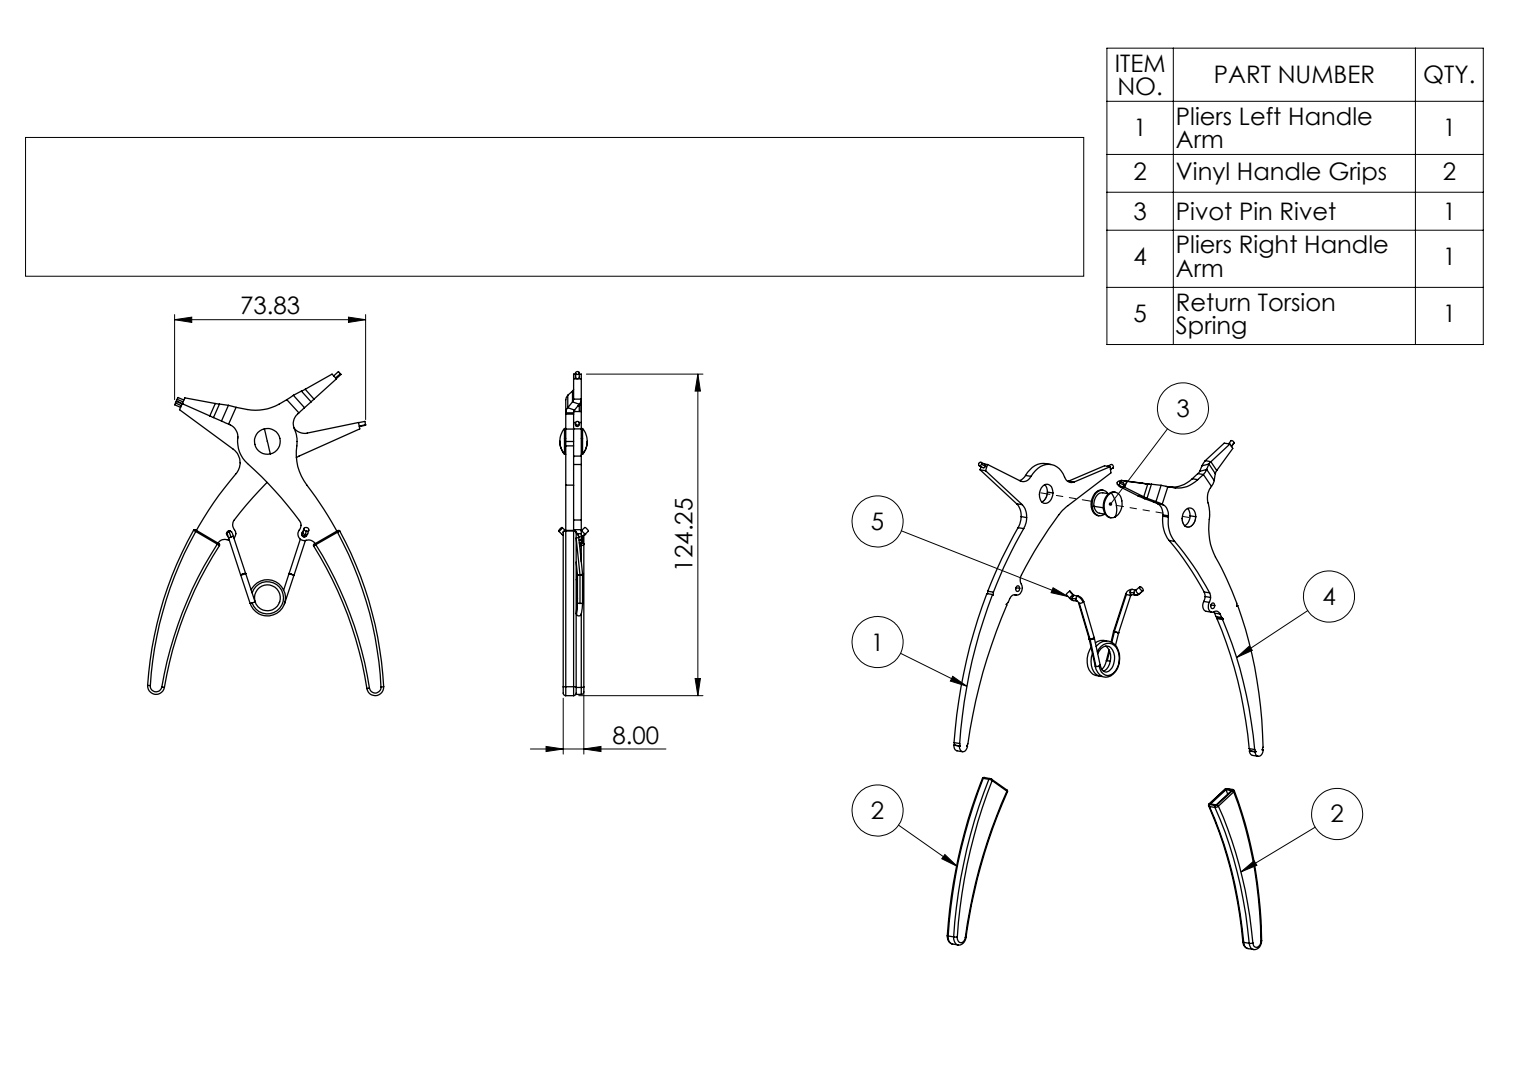
ISO-10303-21;
HEADER;
FILE_DESCRIPTION (('STEP AP214'),
    '1' );
FILE_NAME ('MAS-689',
    '2026-10-09T15:01:35',
    ( '' ),
    ( '' ),
    'SwSTEP 2.0',
    'SolidWorks 2026',
    '' );
FILE_SCHEMA (( 'AUTOMOTIVE_DESIGN' ));
ENDSEC;

DATA;
#1 = ORIENTED_EDGE ( 'NONE', *, *, #451, .F. ) ;
#2 = CIRCLE ( 'NONE', #2039, 3.300000000000002931 ) ;
#3 = DIRECTION ( 'NONE',  ( -5.715354789860003484E-18, -9.999836672264337477E-16, 1.000000000000000000 ) ) ;
#4 = DIRECTION ( 'NONE',  ( -5.715354789860003484E-18, -9.999836672264337477E-16, 1.000000000000000000 ) ) ;
#5 = EDGE_CURVE ( 'NONE', #1930, #3517, #6589, .T. ) ;
#6 = CARTESIAN_POINT ( 'NONE',  ( -2.243961179877913104, -65.88814609558559710, 1.271710548130833951 ) ) ;
#7 = VECTOR ( 'NONE', #4583, 1000.000000000000227 ) ;
#8 = CARTESIAN_POINT ( 'NONE',  ( 7.059059989562619819, -58.43975188330606585, -0.3221438859163246460 ) ) ;
#9 = CARTESIAN_POINT ( 'NONE',  ( -105.7473861751082040, -118.0666774205683822, -1.188285581044112860E-13 ) ) ;
#10 = ORIENTED_EDGE ( 'NONE', *, *, #1499, .F. ) ;
#11 = CARTESIAN_POINT ( 'NONE',  ( 39.48483786921892857, -95.33781693134928048, -9.497611030973018842E-14 ) ) ;
#12 = CARTESIAN_POINT ( 'NONE',  ( 1.714606436958001585E-17, 2.999951001679301835E-15, -3.000000000000000888 ) ) ;
#13 = CARTESIAN_POINT ( 'NONE',  ( 37.74350889372263396, 7.597106414893625370, -1.944871132915118705 ) ) ;
#14 = CARTESIAN_POINT ( 'NONE',  ( 10.02759472486470926, 5.630039434485818894, -2.999999999999995115 ) ) ;
#15 = EDGE_CURVE ( 'NONE', #320, #2542, #2080, .T. ) ;
#16 = CARTESIAN_POINT ( 'NONE',  ( 2.533447467746755333, -55.76293992159236979, -0.1309777151760100067 ) ) ;
#17 = CARTESIAN_POINT ( 'NONE',  ( -31.91091272472834817, 16.82560631625344172, 0.006154456448481410852 ) ) ;
#18 = FACE_OUTER_BOUND ( 'NONE', #7281, .T. ) ;
#19 = CIRCLE ( 'NONE', #5075, 1.000000000000001110 ) ;
#20 = PRODUCT_RELATED_PRODUCT_CATEGORY ( 'part', '', ( #4771 ) ) ;
#21 = ORIENTED_EDGE ( 'NONE', *, *, #345, .T. ) ;
#22 = ORIENTED_EDGE ( 'NONE', *, *, #4795, .T. ) ;
#23 = LINE ( 'NONE', #5799, #7366 ) ;
#24 = AXIS2_PLACEMENT_3D ( 'NONE', #2832, #2306, #6237 ) ;
#25 = AXIS2_PLACEMENT_3D ( 'NONE', #4428, #5501, #4998 ) ;
#26 = LINE ( 'NONE', #2324, #1475 ) ;
#27 = EDGE_CURVE ( 'NONE', #7442, #6679, #395, .T. ) ;
#28 = ADVANCED_FACE ( 'NONE', ( #2146 ), #5063, .T. ) ;
#29 = CARTESIAN_POINT ( 'NONE',  ( -6.272953878096410030, -61.45586155529391448, 1.493064301322690968 ) ) ;
#30 = CARTESIAN_POINT ( 'NONE',  ( 27.63595919327375938, -34.25856858997740062, -0.5081525913518375459 ) ) ;
#31 = CARTESIAN_POINT ( 'NONE',  ( 1.597826897138040048, -55.24069855439622501, 0.3109211183784004184 ) ) ;
#32 = CIRCLE ( 'NONE', #2308, 1.000000000000001110 ) ;
#33 = ORIENTED_EDGE ( 'NONE', *, *, #2628, .F. ) ;
#34 = AXIS2_PLACEMENT_3D ( 'NONE', #6184, #972, #7294 ) ;
#35 = FACE_OUTER_BOUND ( 'NONE', #4506, .T. ) ;
#36 = CARTESIAN_POINT ( 'NONE',  ( -15.08175531864075047, -34.71610473016205134, -5.729623873133089518 ) ) ;
#37 = AXIS2_PLACEMENT_3D ( 'NONE', #1867, #698, #7061 ) ;
#38 = EDGE_CURVE ( 'NONE', #489, #1005, #19, .T. ) ;
#39 = CARTESIAN_POINT ( 'NONE',  ( 9.311407240687648468, -51.41373841511902043, -1.002481404894999928 ) ) ;
#40 = AXIS2_PLACEMENT_3D ( 'NONE', #4287, #3708, #845 ) ;
#41 = CARTESIAN_POINT ( 'NONE',  ( -7.922926035662746003, 12.41525034409755612, 2.701156757981117984 ) ) ;
#42 = CYLINDRICAL_SURFACE ( 'NONE', #5055, 2.999999999999999556 ) ;
#43 = FILL_AREA_STYLE_COLOUR ( '', #963 ) ;
#44 = AXIS2_PLACEMENT_3D ( 'NONE', #1509, #3865, #2736 ) ;
#45 = ORIENTED_EDGE ( 'NONE', *, *, #3432, .T. ) ;
#46 = ORIENTED_EDGE ( 'NONE', *, *, #4272, .T. ) ;
#47 = AXIS2_PLACEMENT_3D ( 'NONE', #6946, #1636, #2269 ) ;
#48 = AXIS2_PLACEMENT_3D ( 'NONE', #1305, #1866, #2469 ) ;
#49 = DIRECTION ( 'NONE',  ( 5.715354789845005112E-18, 9.999836672264339449E-16, -1.000000000000000000 ) ) ;
#50 = AXIS2_PLACEMENT_3D ( 'NONE', #2705, #5732, #561 ) ;
#51 = SURFACE_STYLE_USAGE ( .BOTH. , #5819 ) ;
#52 = DIRECTION ( 'NONE',  ( 0.000000000000000000, -1.000000000000000000, -9.973300763855647239E-16 ) ) ;
#53 = CARTESIAN_POINT ( 'NONE',  ( -28.22553731214382111, -35.79092421365019305, -3.595165860846261460E-14 ) ) ;
#54 = CARTESIAN_POINT ( 'NONE',  ( -1.794944750655344867, -54.19869589391355191, -2.224588173883939035 ) ) ;
#55 = CARTESIAN_POINT ( 'NONE',  ( -13.19674249314596892, -2.997380612392111843, -3.000000000000003997 ) ) ;
#56 = VECTOR ( 'NONE', #5489, 1000.000000000000000 ) ;
#57 = EDGE_LOOP ( 'NONE', ( #3083, #4276, #3063, #5016, #4331, #6608 ) ) ;
#58 = CARTESIAN_POINT ( 'NONE',  ( -15.00216760413269945, 6.625337177075938833, -3.299999999999993161 ) ) ;
#59 = CARTESIAN_POINT ( 'NONE',  ( -14.70408710852078116, -35.66654345889202204, -3.000000000000036415 ) ) ;
#60 = CARTESIAN_POINT ( 'NONE',  ( 17.88843813672053074, -40.41242482140540204, -4.025211077939831437E-14 ) ) ;
#61 = DIRECTION ( 'NONE',  ( -0.9999836672264333925, 0.005715354789844476896, 0.000000000000000000 ) ) ;
#62 = CARTESIAN_POINT ( 'NONE',  ( 3.116905194451685013, -55.41725085606579171, 2.344137946175070653 ) ) ;
#63 = DIRECTION ( 'NONE',  ( -5.715354789860003484E-18, -9.999836672264337477E-16, 1.000000000000000000 ) ) ;
#64 = CARTESIAN_POINT ( 'NONE',  ( 43.95774332523846795, -95.00278575785266355, -9.454242944073598665E-14 ) ) ;
#65 = ORIENTED_EDGE ( 'NONE', *, *, #2017, .F. ) ;
#66 = ORIENTED_EDGE ( 'NONE', *, *, #4521, .T. ) ;
#67 = ORIENTED_EDGE ( 'NONE', *, *, #4872, .T. ) ;
#68 = ADVANCED_FACE ( 'NONE', ( #2687 ), #435, .T. ) ;
#69 = CARTESIAN_POINT ( 'NONE',  ( 18.49916120972752154, -39.46430250869199341, 3.499999999999960476 ) ) ;
#70 = VERTEX_POINT ( 'NONE', #2112 ) ;
#71 = CARTESIAN_POINT ( 'NONE',  ( 1.531562167974070077, -54.12800115838471271, -2.047325108518057935 ) ) ;
#72 = CARTESIAN_POINT ( 'NONE',  ( 26.87031364676133194, -34.69479876584122024, -0.5000000000000345279 ) ) ;
#73 = CARTESIAN_POINT ( 'NONE',  ( 3.016248221826935083, -64.97666327952782694, -3.135076956698916728 ) ) ;
#74 = VERTEX_POINT ( 'NONE', #2232 ) ;
#75 = VERTEX_POINT ( 'NONE', #4424 ) ;
#76 = EDGE_CURVE ( 'NONE', #70, #4585, #6096, .T. ) ;
#77 = EDGE_CURVE ( 'NONE', #427, #2020, #919, .T. ) ;
#78 =( NAMED_UNIT ( * ) SI_UNIT ( $, .STERADIAN. ) SOLID_ANGLE_UNIT ( ) );
#79 = CARTESIAN_POINT ( 'NONE',  ( 12.48153656191966476, 18.70005575237079043, -2.479608496603234347 ) ) ;
#80 = CARTESIAN_POINT ( 'NONE',  ( 8.409045811045761099, -50.95764513735950629, -2.495037190209991707 ) ) ;
#81 = DIRECTION ( 'NONE',  ( -5.715354789845005112E-18, -9.999836672264339449E-16, 1.000000000000000000 ) ) ;
#82 = DIRECTION ( 'NONE',  ( -0.9721221936972339606, -0.2344748185227520099, 0.000000000000000000 ) ) ;
#83 = LINE ( 'NONE', #2969, #2404 ) ;
#84 = EDGE_CURVE ( 'NONE', #5434, #6822, #3844, .T. ) ;
#85 = CARTESIAN_POINT ( 'NONE',  ( -4.132930949989339631, -63.16624423302310021, 2.163545901557570428 ) ) ;
#86 = DIRECTION ( 'NONE',  ( -0.5224671166576538850, 0.8526594349512809368, 0.000000000000000000 ) ) ;
#87 = FACE_OUTER_BOUND ( 'NONE', #3155, .T. ) ;
#88 = CYLINDRICAL_SURFACE ( 'NONE', #3600, 147.0000000000000284 ) ;
#89 = VERTEX_POINT ( 'NONE', #7308 ) ;
#90 = ADVANCED_FACE ( 'NONE', ( #990 ), #3285, .T. ) ;
#91 = CARTESIAN_POINT ( 'NONE',  ( 18.31438873653245381, -40.15745658308031807, 3.873766277856072193 ) ) ;
#92 = CARTESIAN_POINT ( 'NONE',  ( 9.769309212388114005, 25.48802373141157673, -2.993845543551514776 ) ) ;
#93 = FACE_OUTER_BOUND ( 'NONE', #5404, .T. ) ;
#94 = CARTESIAN_POINT ( 'NONE',  ( -2.961840227416660198, -65.56364223063081909, 1.283932781279834900 ) ) ;
#95 = CARTESIAN_POINT ( 'NONE',  ( -1.892846266465454841, -54.28526762408564110, -0.1610563749503846620 ) ) ;
#96 = CARTESIAN_POINT ( 'NONE',  ( 30.52077159997833533, 5.488396937353885896, -1.499999999999994893 ) ) ;
#97 = ORIENTED_EDGE ( 'NONE', *, *, #2305, .F. ) ;
#98 = ORIENTED_EDGE ( 'NONE', *, *, #6789, .F. ) ;
#99 =( REPRESENTATION_RELATIONSHIP ('NONE','NONE', #3195, #2136 ) REPRESENTATION_RELATIONSHIP_WITH_TRANSFORMATION ( #3447 )SHAPE_REPRESENTATION_RELATIONSHIP( ) );
#100 = DIRECTION ( 'NONE',  ( -0.9999836672264332815, 0.005715354789859956701, 0.000000000000000000 ) ) ;
#101 = PLANE ( 'NONE',  #156 ) ;
#102 = CARTESIAN_POINT ( 'NONE',  ( 2.906897738665179975, -66.25564029441702019, 0.8681355557765302322 ) ) ;
#103 = DIRECTION ( 'NONE',  ( 0.2223191033124284066, 0.6712482523644728305, 0.7071067811865467956 ) ) ;
#104 = EDGE_CURVE ( 'NONE', #5945, #4359, #7121, .T. ) ;
#105 = ORIENTED_EDGE ( 'NONE', *, *, #119, .T. ) ;
#106 = VERTEX_POINT ( 'NONE', #6746 ) ;
#107 = CARTESIAN_POINT ( 'NONE',  ( 27.99155020439382469, -34.64269665048638558, -3.446982116472166490E-14 ) ) ;
#108 = DIRECTION ( 'NONE',  ( 0.2344748185227520099, -0.9721221936972339606, 0.000000000000000000 ) ) ;
#109 = CARTESIAN_POINT ( 'NONE',  ( 5.682346379326408403, -62.38461083188095557, -3.511065069215000278 ) ) ;
#110 = DIRECTION ( 'NONE',  ( -0.9721221936972339606, -0.2344748185227520099, 0.000000000000000000 ) ) ;
#111 = EDGE_CURVE ( 'NONE', #70, #3385, #1232, .T. ) ;
#112 = EDGE_CURVE ( 'NONE', #2053, #3816, #7103, .T. ) ;
#113 = CARTESIAN_POINT ( 'NONE',  ( 1.437675307311687245, -54.36893612802973763, 0.01823407963783662405 ) ) ;
#114 = ORIENTED_EDGE ( 'NONE', *, *, #332, .F. ) ;
#115 = PRODUCT_RELATED_PRODUCT_CATEGORY ( 'part', '', ( #196 ) ) ;
#116 = CARTESIAN_POINT ( 'NONE',  ( 4.115360779042029904, -63.19255852436059229, -2.695130055691413506 ) ) ;
#117 = CARTESIAN_POINT ( 'NONE',  ( -20.16480223318149356, 14.61937842657788345, -2.993845543551524990 ) ) ;
#118 = CARTESIAN_POINT ( 'NONE',  ( 9.769309212388092689, 25.48802373141157318, 0.006154456448490518150 ) ) ;
#119 = EDGE_CURVE ( 'NONE', #427, #4029, #5685, .T. ) ;
#120 = ADVANCED_FACE ( 'NONE', ( #5785 ), #4047, .F. ) ;
#121 = CARTESIAN_POINT ( 'NONE',  ( 2.653562475325737857, -65.64394347387724338, 0.9832085570212988346 ) ) ;
#122 = AXIS2_PLACEMENT_3D ( 'NONE', #4190, #238, #5631 ) ;
#123 = VERTEX_POINT ( 'NONE', #4619 ) ;
#124 = CARTESIAN_POINT ( 'NONE',  ( -5.765066695091211280, -62.35357808832723947, 3.545399627195713332 ) ) ;
#125 = AXIS2_PLACEMENT_3D ( 'NONE', #6895, #3541, #4566 ) ;
#126 = DIRECTION ( 'NONE',  ( -0.2344748185227520376, 0.9721221936972340716, 0.000000000000000000 ) ) ;
#127 = CARTESIAN_POINT ( 'NONE',  ( 1.275220786007323914, -54.66846601681689322, 0.1350250863793004130 ) ) ;
#128 = CARTESIAN_POINT ( 'NONE',  ( 2.080482015124565098, -66.54183146390657555, -1.221303033644861813 ) ) ;
#129 = DIRECTION ( 'NONE',  ( -1.602374898470634869E-16, 1.442524254523139935E-17, 1.000000000000000000 ) ) ;
#130 = ORIENTED_EDGE ( 'NONE', *, *, #2556, .T. ) ;
#131 = ORIENTED_EDGE ( 'NONE', *, *, #84, .F. ) ;
#132 = VECTOR ( 'NONE', #4275, 1000.000000000000000 ) ;
#133 = FACE_OUTER_BOUND ( 'NONE', #7338, .T. ) ;
#134 = CARTESIAN_POINT ( 'NONE',  ( -4.860610968486169803, -1.172374092613760022, 3.500000000000000000 ) ) ;
#135 = CARTESIAN_POINT ( 'NONE',  ( -6.814417183322500016, -58.48210382454914935, -0.1019614231452001113 ) ) ;
#136 = CARTESIAN_POINT ( 'NONE',  ( 27.99155020439386377, -34.64269665048637137, -4.257530847521587323E-14 ) ) ;
#137 = ORIENTED_EDGE ( 'NONE', *, *, #2521, .F. ) ;
#138 = VERTEX_POINT ( 'NONE', #4690 ) ;
#139 = ORIENTED_EDGE ( 'NONE', *, *, #2264, .T. ) ;
#140 = EDGE_CURVE ( 'NONE', #6822, #6113, #1025, .T. ) ;
#141 =( NAMED_UNIT ( * ) SI_UNIT ( $, .STERADIAN. ) SOLID_ANGLE_UNIT ( ) );
#142 = PLANE ( 'NONE',  #2794 ) ;
#143 = DIRECTION ( 'NONE',  ( -0.9721221936972339606, -0.2344748185227520099, 0.000000000000000000 ) ) ;
#144 = DIRECTION ( 'NONE',  ( 0.2223157560262044585, -0.6712493609847989262, 0.7071067811865449082 ) ) ;
#145 = CARTESIAN_POINT ( 'NONE',  ( 30.52077159997833533, 5.488396937353885896, -1.499999999999994893 ) ) ;
#146 = CIRCLE ( 'NONE', #7235, 1.000000000000000888 ) ;
#147 = CIRCLE ( 'NONE', #6885, 6.299999999999998934 ) ;
#148 = AXIS2_PLACEMENT_3D ( 'NONE', #6165, #6059, #1524 ) ;
#149 = CARTESIAN_POINT ( 'NONE',  ( -5.163597282883630513, -63.01551968439245144, 3.580859834736030312 ) ) ;
#150 = VECTOR ( 'NONE', #1771, 1000.000000000000227 ) ;
#151 = VECTOR ( 'NONE', #4371, 999.9999999999998863 ) ;
#152 = CARTESIAN_POINT ( 'NONE',  ( 0.000000000000000000, 0.000000000000000000, 2.544444444444450060 ) ) ;
#153 = CARTESIAN_POINT ( 'NONE',  ( -4.969000869418408683, -63.40403411709974790, -2.714243491562927879 ) ) ;
#154 = CARTESIAN_POINT ( 'NONE',  ( -2.104778383727555102, -66.59261038346899397, 1.133408834283370137 ) ) ;
#155 = DIRECTION ( 'NONE',  ( -0.9999836672264332815, 0.005715354789859956701, 0.000000000000000000 ) ) ;
#156 = AXIS2_PLACEMENT_3D ( 'NONE', #5801, #629, #4670 ) ;
#157 = CIRCLE ( 'NONE', #1946, 1.000000000000000444 ) ;
#158 = EDGE_LOOP ( 'NONE', ( #2587, #5336, #2767, #4336, #3455, #7221 ) ) ;
#159 = PRODUCT_DEFINITION_FORMATION_WITH_SPECIFIED_SOURCE ( 'ANY', '', #255, .NOT_KNOWN. ) ;
#160 = CARTESIAN_POINT ( 'NONE',  ( -28.26642576027046516, -36.90973657692984489, -3.000000000000037748 ) ) ;
#161 = EDGE_CURVE ( 'NONE', #2317, #4548, #3992, .T. ) ;
#162 = EDGE_CURVE ( 'NONE', #6490, #232, #2554, .T. ) ;
#163 = LINE ( 'NONE', #7048, #1585 ) ;
#164 = AXIS2_PLACEMENT_3D ( 'NONE', #6562, #6008, #5019 ) ;
#165 = CARTESIAN_POINT ( 'NONE',  ( 12.40979888490706706, -30.61452125107581068, 2.999999999999969802 ) ) ;
#166 = DIRECTION ( 'NONE',  ( 5.715354789845005112E-18, 9.999836672264339449E-16, -1.000000000000000000 ) ) ;
#167 = CARTESIAN_POINT ( 'NONE',  ( -6.199032880790720235, -61.56120177486793210, 3.556545127952429830 ) ) ;
#168 = AXIS2_PLACEMENT_3D ( 'NONE', #4159, #3722, #2491 ) ;
#169 = CIRCLE ( 'NONE', #2691, 147.0000000000000000 ) ;
#170 = CARTESIAN_POINT ( 'NONE',  ( 5.465222000274489567, -57.03231251543625291, 0.2812537129946697800 ) ) ;
#171 = CARTESIAN_POINT ( 'NONE',  ( -16.51707533432788111, -40.85914143033993895, -3.000000000000041744 ) ) ;
#172 = ORIENTED_EDGE ( 'NONE', *, *, #3864, .T. ) ;
#173 = ORIENTED_EDGE ( 'NONE', *, *, #526, .F. ) ;
#174 = ORIENTED_EDGE ( 'NONE', *, *, #2963, .T. ) ;
#175 = EDGE_CURVE ( 'NONE', #6662, #3589, #2174, .T. ) ;
#176 = CIRCLE ( 'NONE', #6665, 0.7499999999999893419 ) ;
#177 = DIRECTION ( 'NONE',  ( -0.9492883822130750993, 0.3144066910790588865, 0.000000000000000000 ) ) ;
#178 = PLANE ( 'NONE',  #37 ) ;
#179 = CARTESIAN_POINT ( 'NONE',  ( 5.575556491096470779, -57.10417477796837460, -1.782215851858570010 ) ) ;
#180 = CARTESIAN_POINT ( 'NONE',  ( 9.311407240687648468, -51.41373841511900622, -2.502481404895003259 ) ) ;
#181 = VERTEX_POINT ( 'NONE', #5749 ) ;
#182 = ORIENTED_EDGE ( 'NONE', *, *, #4904, .T. ) ;
#183 = ORIENTED_EDGE ( 'NONE', *, *, #2628, .T. ) ;
#184 = VERTEX_POINT ( 'NONE', #578 ) ;
#185 =( LENGTH_UNIT ( ) NAMED_UNIT ( * ) SI_UNIT ( .MILLI., .METRE. ) );
#186 = CARTESIAN_POINT ( 'NONE',  ( 3.888488774788935842, 0.9378992740910084835, 3.000000000000000000 ) ) ;
#187 = CARTESIAN_POINT ( 'NONE',  ( 27.98760434640042050, 26.43260972569849443, -1.493845543551990174 ) ) ;
#188 = DIRECTION ( 'NONE',  ( 0.3128416502900965290, -0.9445788350777319931, 0.09950339776592478924 ) ) ;
#189 = CARTESIAN_POINT ( 'NONE',  ( -3.569041007005829602, -65.81017109676685095, 3.284668648760890264 ) ) ;
#190 = PLANE ( 'NONE',  #25 ) ;
#191 = ORIENTED_EDGE ( 'NONE', *, *, #892, .F. ) ;
#192 = CARTESIAN_POINT ( 'NONE',  ( -2.392055737067099841, -65.19778216667813808, -1.190937291917544050 ) ) ;
#193 = CARTESIAN_POINT ( 'NONE',  ( -14.49899450467539985, -35.75040780681265318, -0.4662714048949997969 ) ) ;
#194 = DIRECTION ( 'NONE',  ( 9.251858538542970644E-15, 2.775557561562891351E-14, 1.000000000000000000 ) ) ;
#195 = CARTESIAN_POINT ( 'NONE',  ( -3.055077159899213690, -65.35589988530520600, -0.7735514844714416194 ) ) ;
#196 = PRODUCT ( 'Pliers Right Handle Arm', 'Pliers Right Handle Arm', '', ( #6070 ) ) ;
#197 = CARTESIAN_POINT ( 'NONE',  ( 3.257640280419950241, -66.06664283717124420, -1.252360977842533751 ) ) ;
#198 = EDGE_CURVE ( 'NONE', #3368, #5232, #6974, .T. ) ;
#199 = ORIENTED_EDGE ( 'NONE', *, *, #978, .F. ) ;
#200 = DIRECTION ( 'NONE',  ( 0.9999836672264332815, -0.005715354789844959149, 0.000000000000000000 ) ) ;
#201 = DIRECTION ( 'NONE',  ( 0.8552446107963830313, 0.5182245224839744369, 5.231040848230092092E-16 ) ) ;
#202 = CYLINDRICAL_SURFACE ( 'NONE', #2445, 0.5000000000000022204 ) ;
#203 = CARTESIAN_POINT ( 'NONE',  ( -3.235261603508409856, -66.01500717273368934, 1.164464255201294929 ) ) ;
#204 = CARTESIAN_POINT ( 'NONE',  ( -5.227302941343250353, -58.92678856866081105, -0.2192372590660296439 ) ) ;
#205 = CARTESIAN_POINT ( 'NONE',  ( -6.490403473174280791, -62.28500686936251185, 3.403714661497959870 ) ) ;
#206 = EDGE_CURVE ( 'NONE', #2991, #6689, #4958, .T. ) ;
#207 = CARTESIAN_POINT ( 'NONE',  ( -17.21006346072928750, 13.86884027412869180, -2.230393353321906247 ) ) ;
#208 = ORIENTED_EDGE ( 'NONE', *, *, #252, .F. ) ;
#209 = ADVANCED_FACE ( 'NONE', ( #688 ), #379, .F. ) ;
#210 = VERTEX_POINT ( 'NONE', #2865 ) ;
#211 = EDGE_LOOP ( 'NONE', ( #3520, #3050, #137, #3824 ) ) ;
#212 = VERTEX_POINT ( 'NONE', #11 ) ;
#213 = DIRECTION ( 'NONE',  ( -5.715354789845005112E-18, -9.999836672264339449E-16, 1.000000000000000000 ) ) ;
#214 = CARTESIAN_POINT ( 'NONE',  ( 14.18471095241310032, -36.69976849081635351, 0.4975185951050001831 ) ) ;
#215 = CARTESIAN_POINT ( 'NONE',  ( -1.756031117750795234, -65.59594772693552045, 1.371125244074580030 ) ) ;
#216 = VERTEX_POINT ( 'NONE', #6910 ) ;
#217 = EDGE_CURVE ( 'NONE', #3483, #2618, #2661, .T. ) ;
#218 = ORIENTED_EDGE ( 'NONE', *, *, #3975, .F. ) ;
#219 = EDGE_LOOP ( 'NONE', ( #5454, #1451, #6530, #3936 ) ) ;
#220 = ORIENTED_EDGE ( 'NONE', *, *, #5909, .F. ) ;
#221 = DIRECTION ( 'NONE',  ( 0.1200071523045019850, -0.5808948794702039065, -0.8050834878452428622 ) ) ;
#222 = CARTESIAN_POINT ( 'NONE',  ( 27.68174825049008803, -37.24611774345110859, -3.729655473350135253E-14 ) ) ;
#223 = DIRECTION ( 'NONE',  ( 0.4039838799357178822, 0.9147661038495488173, -2.999999999999999208E-14 ) ) ;
#224 = CARTESIAN_POINT ( 'NONE',  ( -6.308476396955129850, -59.14191327212131455, -0.5142043607924547954 ) ) ;
#225 = ORIENTED_EDGE ( 'NONE', *, *, #2234, .T. ) ;
#226 = EDGE_CURVE ( 'NONE', #477, #1089, #6052, .T. ) ;
#227 = DIRECTION ( 'NONE',  ( 5.715354789845004342E-18, 9.999836672264337477E-16, -1.000000000000000000 ) ) ;
#228 = CARTESIAN_POINT ( 'NONE',  ( -5.725946002089390419, -61.92844332740136792, 1.548851071596535123 ) ) ;
#229 =( NAMED_UNIT ( * ) SI_UNIT ( $, .STERADIAN. ) SOLID_ANGLE_UNIT ( ) );
#230 = DIRECTION ( 'NONE',  ( -0.9999836672264333925, 0.005715354789844960016, 0.000000000000000000 ) ) ;
#231 = CARTESIAN_POINT ( 'NONE',  ( 2.221695044209367698, -65.89517911169727427, -1.088420971642926727 ) ) ;
#232 = VERTEX_POINT ( 'NONE', #3010 ) ;
#233 = LINE ( 'NONE', #4722, #5692 ) ;
#234 = TOROIDAL_SURFACE ( 'NONE', #5408, 140.0000000000000000, 1.000000000000000000 ) ;
#235 = EDGE_CURVE ( 'NONE', #5505, #4310, #421, .T. ) ;
#236 = CARTESIAN_POINT ( 'NONE',  ( -19.02987527034469650, -39.22028924617138301, -3.000000000000040412 ) ) ;
#237 = CARTESIAN_POINT ( 'NONE',  ( 18.49916120972751088, -39.46430250869199341, -0.5000000000000393019 ) ) ;
#238 = DIRECTION ( 'NONE',  ( 0.6713653717953971256, -0.7411265327553914206, -1.050567784676125892E-15 ) ) ;
#239 = CARTESIAN_POINT ( 'NONE',  ( -6.429839020462739363, -63.58404662519255623, 2.770540757372710328 ) ) ;
#240 = CARTESIAN_POINT ( 'NONE',  ( -44.78727511552453677, -94.39397278840091587, -9.464840624037363205E-14 ) ) ;
#241 = EDGE_LOOP ( 'NONE', ( #2453, #5652, #2656, #1275 ) ) ;
#242 = ORIENTED_EDGE ( 'NONE', *, *, #3196, .T. ) ;
#243 = AXIS2_PLACEMENT_3D ( 'NONE', #3684, #2023, #7044 ) ;
#244 = CARTESIAN_POINT ( 'NONE',  ( -28.68093632328499965, 11.79168739492699913, -1.500000000001999956 ) ) ;
#245 = CARTESIAN_POINT ( 'NONE',  ( -105.7473861751082040, -118.0666774205683822, 2.999999999999881428 ) ) ;
#246 = CARTESIAN_POINT ( 'NONE',  ( -5.466570931786790766, -63.95713299600960511, -2.842748680216657942 ) ) ;
#247 = CARTESIAN_POINT ( 'NONE',  ( 2.831152723192955190, -54.81765481733766876, 0.09675599308719184943 ) ) ;
#248 = CIRCLE ( 'NONE', #4943, 5.000000000000001776 ) ;
#249 = ORIENTED_EDGE ( 'NONE', *, *, #5609, .F. ) ;
#250 = EDGE_LOOP ( 'NONE', ( #2222, #4590, #6016, #4607 ) ) ;
#251 = ORIENTED_EDGE ( 'NONE', *, *, #6437, .T. ) ;
#252 = EDGE_CURVE ( 'NONE', #1688, #1547, #147, .T. ) ;
#253 = EDGE_CURVE ( 'NONE', #4908, #2830, #5444, .T. ) ;
#254 = CARTESIAN_POINT ( 'NONE',  ( 23.12979183812720407, 24.32586137474685017, -8.815182418718713109 ) ) ;
#255 = PRODUCT ( 'Return Torsion Spring', 'Return Torsion Spring', '', ( #964 ) ) ;
#256 = FACE_BOUND ( 'NONE', #7433, .T. ) ;
#257 = CARTESIAN_POINT ( 'NONE',  ( 12.34225220476766438, -34.27182074065601114, 2.999999999999965805 ) ) ;
#258 = CARTESIAN_POINT ( 'NONE',  ( -5.971666637568279867, -56.84728173661435591, 1.574849794282134896 ) ) ;
#259 = ORIENTED_EDGE ( 'NONE', *, *, #1801, .T. ) ;
#260 = DIRECTION ( 'NONE',  ( -0.6713653717953970146, 0.7411265327553913096, 7.633377738797892154E-16 ) ) ;
#261 = EDGE_CURVE ( 'NONE', #1236, #2830, #5625, .T. ) ;
#262 = CARTESIAN_POINT ( 'NONE',  ( 4.897692307440769888, -62.02301377339387756, -1.765793165935516829 ) ) ;
#263 = CARTESIAN_POINT ( 'NONE',  ( 12.26605808802378661, -5.710507655519335479, -3.000000000000006661 ) ) ;
#264 = VECTOR ( 'NONE', #2040, 1000.000000000000000 ) ;
#265 = VECTOR ( 'NONE', #2707, 999.9999999999998863 ) ;
#266 = CYLINDRICAL_SURFACE ( 'NONE', #6602, 11.50000000000000178 ) ;
#267 = CARTESIAN_POINT ( 'NONE',  ( 3.367951392835606406, -65.15049214652208320, -1.167130348240442927 ) ) ;
#268 = ORIENTED_EDGE ( 'NONE', *, *, #1200, .T. ) ;
#269 = CIRCLE ( 'NONE', #6408, 140.0000000000000000 ) ;
#270 = CARTESIAN_POINT ( 'NONE',  ( -41.31559769795914150, -94.79889909491285493, -3.000000000000095923 ) ) ;
#271 = VECTOR ( 'NONE', #2311, 1000.000000000000000 ) ;
#272 = DIRECTION ( 'NONE',  ( 0.3128463504745285229, 0.9445772445362839997, 0.09950371902099811039 ) ) ;
#273 = DIRECTION ( 'NONE',  ( -0.4039838799357104993, -0.9147661038495521479, -3.619485620725444841E-16 ) ) ;
#274 = UNCERTAINTY_MEASURE_WITH_UNIT (LENGTH_MEASURE( 1.000000000000000082E-05 ), #185, 'distance_accuracy_value', 'NONE');
#275 = AXIS2_PLACEMENT_3D ( 'NONE', #245, #7168, #3592 ) ;
#276 = CARTESIAN_POINT ( 'NONE',  ( -3.156642594714314853, -54.82761582543010093, 1.871643660998590697 ) ) ;
#277 = AXIS2_PLACEMENT_3D ( 'NONE', #4931, #1502, #1047 ) ;
#278 = CARTESIAN_POINT ( 'NONE',  ( -1.626396133375414887, -53.66552156771879112, 1.839959185157149957 ) ) ;
#279 = DIRECTION ( 'NONE',  ( 0.000000000000000000, -0.7252570966694442678, 0.6884781359858920258 ) ) ;
#280 = ORIENTED_EDGE ( 'NONE', *, *, #2225, .T. ) ;
#281 = AXIS2_PLACEMENT_3D ( 'NONE', #1500, #409, #4895 ) ;
#282 = ORIENTED_EDGE ( 'NONE', *, *, #5430, .F. ) ;
#283 = ORIENTED_EDGE ( 'NONE', *, *, #2017, .T. ) ;
#284 = AXIS2_PLACEMENT_3D ( 'NONE', #2458, #4271, #126 ) ;
#285 = CARTESIAN_POINT ( 'NONE',  ( -15.07233531785332659, 13.90759097395377886, 2.236547809770392803 ) ) ;
#286 = CIRCLE ( 'NONE', #4504, 147.0000000000000284 ) ;
#287 = VECTOR ( 'NONE', #7438, 1000.000000000000000 ) ;
#288 = DIRECTION ( 'NONE',  ( 0.9986925448795970217, 0.05111947575938272093, 5.682652305652042775E-17 ) ) ;
#289 = CARTESIAN_POINT ( 'NONE',  ( 1.662636012147085118, -65.62619303409478277, -3.045852711070930141 ) ) ;
#290 = CARTESIAN_POINT ( 'NONE',  ( 4.774359225188401723, -64.47360709931102463, 0.6998940494460414996 ) ) ;
#291 = ORIENTED_EDGE ( 'NONE', *, *, #6437, .F. ) ;
#292 = ORIENTED_EDGE ( 'NONE', *, *, #6726, .T. ) ;
#293 = EDGE_CURVE ( 'NONE', #961, #6756, #1329, .T. ) ;
#294 = ORIENTED_EDGE ( 'NONE', *, *, #1501, .T. ) ;
#295 = ORIENTED_EDGE ( 'NONE', *, *, #5689, .F. ) ;
#296 = DIRECTION ( 'NONE',  ( 0.9492899500389736511, 0.3144019573014823488, 0.000000000000000000 ) ) ;
#297 = DIRECTION ( 'NONE',  ( -0.2023178344681509366, 0.9793199139485104787, 9.781476007338054812E-16 ) ) ;
#298 = CIRCLE ( 'NONE', #3775, 145.9999999999999716 ) ;
#299 = PLANE ( 'NONE',  #650 ) ;
#300 = CARTESIAN_POINT ( 'NONE',  ( 6.696612653858620590, -58.50870383553881737, 0.2496331057155200817 ) ) ;
#301 = EDGE_LOOP ( 'NONE', ( #225, #3972, #6636, #4802 ) ) ;
#302 = ADVANCED_FACE ( 'NONE', ( #3614 ), #3261, .F. ) ;
#303 = EDGE_CURVE ( 'NONE', #4768, #4244, #4606, .T. ) ;
#304 = EDGE_LOOP ( 'NONE', ( #2533, #3781, #4954, #1609 ) ) ;
#305 = DIRECTION ( 'NONE',  ( 5.715354789845005112E-18, 9.999836672264339449E-16, -1.000000000000000000 ) ) ;
#306 = CARTESIAN_POINT ( 'NONE',  ( -5.408997660349871062, -62.29959681528816873, 3.625047998704080232 ) ) ;
#307 = ORIENTED_EDGE ( 'NONE', *, *, #6778, .T. ) ;
#308 = DIRECTION ( 'NONE',  ( -5.715354789860003484E-18, -9.999836672264337477E-16, 1.000000000000000000 ) ) ;
#309 = CARTESIAN_POINT ( 'NONE',  ( -0.5318364440386327274, -66.20751837745356738, -3.028967907328838027 ) ) ;
#310 = EDGE_CURVE ( 'NONE', #1930, #1079, #233, .T. ) ;
#311 = ORIENTED_EDGE ( 'NONE', *, *, #217, .T. ) ;
#312 = CARTESIAN_POINT ( 'NONE',  ( 14.02750760687355935, -37.17441268192290238, 0.4975185951050001831 ) ) ;
#313 = CARTESIAN_POINT ( 'NONE',  ( 27.55235279947361349, -34.88166451341158592, 3.999999999999965361 ) ) ;
#314 = DIRECTION ( 'NONE',  ( 0.3128416502900965290, -0.9445788350777319931, 0.09950339776592478924 ) ) ;
#315 = DIRECTION ( 'NONE',  ( -0.4328040977884316520, 0.5819352847797604200, 0.6884997728872834788 ) ) ;
#316 = LINE ( 'NONE', #1518, #3268 ) ;
#317 = CARTESIAN_POINT ( 'NONE',  ( 6.075450823322679383, -63.85990335785957228, 0.5148622082158803570 ) ) ;
#318 = CARTESIAN_POINT ( 'NONE',  ( -95.86211798318534250, -102.0316339954322018, 3.999999999999897859 ) ) ;
#319 = ADVANCED_FACE ( 'NONE', ( #794 ), #822, .F. ) ;
#320 = VERTEX_POINT ( 'NONE', #758 ) ;
#321 = VERTEX_POINT ( 'NONE', #1855 ) ;
#322 = CARTESIAN_POINT ( 'NONE',  ( 15.39900769062488806, 3.181283097128406290, -2.999999999999997335 ) ) ;
#323 = FACE_OUTER_BOUND ( 'NONE', #1179, .T. ) ;
#324 = CARTESIAN_POINT ( 'NONE',  ( -4.747117373927349782, -63.10583374278928659, -0.4844647803776696016 ) ) ;
#325 = CARTESIAN_POINT ( 'NONE',  ( 6.103722004628568065, 22.16747290800961778, 2.236547809770398576 ) ) ;
#326 = CARTESIAN_POINT ( 'NONE',  ( -4.385465831998347497, -64.89496069624793506, 1.250664309176121813 ) ) ;
#327 = VERTEX_POINT ( 'NONE', #3117 ) ;
#328 = ORIENTED_EDGE ( 'NONE', *, *, #1145, .T. ) ;
#329 = ORIENTED_EDGE ( 'NONE', *, *, #1529, .F. ) ;
#330 =( NAMED_UNIT ( * ) PLANE_ANGLE_UNIT ( ) SI_UNIT ( $, .RADIAN. ) );
#331 = CARTESIAN_POINT ( 'NONE',  ( -18.51952944085035924, 14.44713361607367830, 0.4060579846639892909 ) ) ;
#332 = EDGE_CURVE ( 'NONE', #5680, #3331, #6168, .T. ) ;
#333 = LINE ( 'NONE', #6030, #1620 ) ;
#334 = CARTESIAN_POINT ( 'NONE',  ( -33.25476684253261794, 13.81160679460555940, -0.7499999999999977796 ) ) ;
#335 = CARTESIAN_POINT ( 'NONE',  ( 1.944327905822930136, -53.75057748617523856, 2.017748614706070143 ) ) ;
#336 = ORIENTED_EDGE ( 'NONE', *, *, #6986, .T. ) ;
#337 = FACE_OUTER_BOUND ( 'NONE', #6918, .T. ) ;
#338 = CARTESIAN_POINT ( 'NONE',  ( -1.512046953658800152, -54.18079592905042574, 1.959428465566195543 ) ) ;
#339 = EDGE_CURVE ( 'NONE', #4174, #2620, #4361, .T. ) ;
#340 = CYLINDRICAL_SURFACE ( 'NONE', #3356, 0.7500000000000000000 ) ;
#341 = DIRECTION ( 'NONE',  ( 5.715354789860003484E-18, 9.999836672264337477E-16, -1.000000000000000000 ) ) ;
#342 = ORIENTED_EDGE ( 'NONE', *, *, #3838, .T. ) ;
#343 = EDGE_CURVE ( 'NONE', #1942, #4478, #3077, .T. ) ;
#344 = CARTESIAN_POINT ( 'NONE',  ( 18.49916120972752509, -39.46430250869199341, 3.499999999999960476 ) ) ;
#345 = EDGE_CURVE ( 'NONE', #1893, #5033, #4794, .T. ) ;
#346 = CYLINDRICAL_SURFACE ( 'NONE', #4266, 3.300000000000001599 ) ;
#347 = DIRECTION ( 'NONE',  ( -0.8056443796264689539, 0.5923994712829191434, 5.877852522924718954E-16 ) ) ;
#348 = DIRECTION ( 'NONE',  ( -5.715354789845005112E-18, -9.999836672264339449E-16, 1.000000000000000000 ) ) ;
#349 = FACE_OUTER_BOUND ( 'NONE', #6871, .T. ) ;
#350 = CARTESIAN_POINT ( 'NONE',  ( 3.592758869166885471, -66.41582265024271692, 0.6922273147611399668 ) ) ;
#351 = DIRECTION ( 'NONE',  ( -5.715354789860003484E-18, -9.999836672264337477E-16, 1.000000000000000000 ) ) ;
#352 = AXIS2_PLACEMENT_3D ( 'NONE', #2407, #3501, #6969 ) ;
#353 = ORIENTED_EDGE ( 'NONE', *, *, #3724, .F. ) ;
#354 = VERTEX_POINT ( 'NONE', #1399 ) ;
#355 = ORIENTED_EDGE ( 'NONE', *, *, #4403, .T. ) ;
#356 = FACE_OUTER_BOUND ( 'NONE', #779, .T. ) ;
#357 = AXIS2_PLACEMENT_3D ( 'NONE', #1661, #431, #1029 ) ;
#358 = FACE_OUTER_BOUND ( 'NONE', #3624, .T. ) ;
#359 = CARTESIAN_POINT ( 'NONE',  ( -5.294444503516980483, -61.70453834742492916, -0.3952116983248150084 ) ) ;
#360 = FACE_OUTER_BOUND ( 'NONE', #2389, .T. ) ;
#361 = CARTESIAN_POINT ( 'NONE',  ( -6.248181790555211279, -60.49255085186674563, 1.512929826500920338 ) ) ;
#362 = CARTESIAN_POINT ( 'NONE',  ( -4.797760869400969241, -62.71499483963494015, 1.636667228454699696 ) ) ;
#363 = ORIENTED_EDGE ( 'NONE', *, *, #858, .F. ) ;
#364 = VERTEX_POINT ( 'NONE', #160 ) ;
#365 = EDGE_LOOP ( 'NONE', ( #2898, #4599, #960, #5000 ) ) ;
#366 = VECTOR ( 'NONE', #3433, 1000.000000000000000 ) ;
#367 =( NAMED_UNIT ( * ) PLANE_ANGLE_UNIT ( ) SI_UNIT ( $, .RADIAN. ) );
#368 = DIRECTION ( 'NONE',  ( 5.715354789845005112E-18, 9.999836672264339449E-16, -1.000000000000000000 ) ) ;
#369 = AXIS2_PLACEMENT_3D ( 'NONE', #2221, #569, #5170 ) ;
#370 = DIRECTION ( 'NONE',  ( -0.9999836672264335036, 0.005715354789845008589, 0.000000000000000000 ) ) ;
#371 = CARTESIAN_POINT ( 'NONE',  ( 6.135463341229070444, -63.36916140199613778, -1.604994752452352014 ) ) ;
#372 = ORIENTED_EDGE ( 'NONE', *, *, #5459, .F. ) ;
#373 = ORIENTED_EDGE ( 'NONE', *, *, #4079, .F. ) ;
#374 = ADVANCED_FACE ( 'NONE', ( #1915 ), #2901, .T. ) ;
#375 = CARTESIAN_POINT ( 'NONE',  ( 39.48483786921892857, -95.33781693134928048, 3.999999999999904521 ) ) ;
#376 = CARTESIAN_POINT ( 'NONE',  ( -18.51952944085035924, 14.44713361607365876, 0.4060579846639944535 ) ) ;
#377 = CARTESIAN_POINT ( 'NONE',  ( 15.08188723176695056, -33.99092340910145538, 5.072392329257909616 ) ) ;
#378 = DIRECTION ( 'NONE',  ( 0.000000000000000000, -0.7252570966694443788, 0.6884781359858918037 ) ) ;
#379 = CONICAL_SURFACE ( 'NONE', #3862, 0.7499999999999865663, 1.029744258676651425 ) ;
#380 = VERTEX_POINT ( 'NONE', #6559 ) ;
#381 = EDGE_CURVE ( 'NONE', #2927, #5703, #3139, .T. ) ;
#382 = B_SPLINE_CURVE_WITH_KNOTS ( 'NONE', 3,
 ( #5287, #6445, #2450, #5362, #4685, #5889 ),
 .UNSPECIFIED., .F., .F.,
 ( 4, 2, 4 ),
 ( 0.000000000000000000, 0.5000000000000000000, 1.000000000000000000 ),
 .UNSPECIFIED. ) ;
#383 = VECTOR ( 'NONE', #1135, 1000.000000000000000 ) ;
#384 = DIRECTION ( 'NONE',  ( 0.9999836672264332815, -0.005715354789859936752, 0.000000000000000000 ) ) ;
#385 = CARTESIAN_POINT ( 'NONE',  ( 7.541408601728222472, 23.46983215994270822, -2.230393353321886263 ) ) ;
#386 = CARTESIAN_POINT ( 'NONE',  ( -105.7473861751082040, -118.0666774205683822, 2.999999999999881428 ) ) ;
#387 = CARTESIAN_POINT ( 'NONE',  ( -95.86211798318534250, -102.0316339954322018, 2.999999999999897859 ) ) ;
#388 = CARTESIAN_POINT ( 'NONE',  ( -6.381106047699259598, -62.60757382768967716, 3.386766328596300113 ) ) ;
#389 = DIRECTION ( 'NONE',  ( 0.000000000000000000, 0.000000000000000000, -1.000000000000000000 ) ) ;
#390 = AXIS2_PLACEMENT_3D ( 'NONE', #1613, #3079, #7288 ) ;
#391 = AXIS2_PLACEMENT_3D ( 'NONE', #5186, #5641, #2797 ) ;
#392 = ORIENTED_EDGE ( 'NONE', *, *, #7416, .F. ) ;
#393 = EDGE_CURVE ( 'NONE', #1414, #6322, #2060, .T. ) ;
#394 = AXIS2_PLACEMENT_3D ( 'NONE', #12, #4824, #4257 ) ;
#395 = LINE ( 'NONE', #4507, #6992 ) ;
#396 = CARTESIAN_POINT ( 'NONE',  ( 14.63724902514210058, -34.60816281716094522, 2.969700630898919780 ) ) ;
#397 = AXIS2_PLACEMENT_3D ( 'NONE', #3733, #472, #2723 ) ;
#398 = AXIS2_PLACEMENT_3D ( 'NONE', #5979, #4800, #4664 ) ;
#399 = DIRECTION ( 'NONE',  ( -5.715354789845005112E-18, -9.999836672264339449E-16, 1.000000000000000000 ) ) ;
#400 = CARTESIAN_POINT ( 'NONE',  ( -4.470547512179178895, -58.04376326654274720, -1.678768375691622960 ) ) ;
#401 = CARTESIAN_POINT ( 'NONE',  ( 27.74785680215192940, -34.19481439742430240, 3.132117371547133100 ) ) ;
#402 = CARTESIAN_POINT ( 'NONE',  ( -4.067320158550557174, -55.70390554630877489, -0.2964418605464455014 ) ) ;
#403 = ORIENTED_EDGE ( 'NONE', *, *, #803, .T. ) ;
#404 = EDGE_CURVE ( 'NONE', #7317, #6686, #1470, .T. ) ;
#405 = ORIENTED_EDGE ( 'NONE', *, *, #2511, .F. ) ;
#406 = ORIENTED_EDGE ( 'NONE', *, *, #5399, .F. ) ;
#407 = AXIS2_PLACEMENT_3D ( 'NONE', #1418, #3070, #5386 ) ;
#408 = CIRCLE ( 'NONE', #6306, 1.000000000000000888 ) ;
#409 = DIRECTION ( 'NONE',  ( 0.000000000000000000, 0.000000000000000000, 1.000000000000000000 ) ) ;
#410 = DIRECTION ( 'NONE',  ( 0.9999836672264332815, -0.005715354789845306094, 0.000000000000000000 ) ) ;
#411 = CARTESIAN_POINT ( 'NONE',  ( -14.70408710852078116, -35.66654345889202204, -3.575000000000001175E-14 ) ) ;
#412 = DIRECTION ( 'NONE',  ( -5.715354789860003484E-18, -9.999836672264337477E-16, 1.000000000000000000 ) ) ;
#413 = FACE_OUTER_BOUND ( 'NONE', #4875, .T. ) ;
#414 = CARTESIAN_POINT ( 'NONE',  ( -3.723298236168965047, -66.76642012610518861, 0.4732191326009700938 ) ) ;
#415 = ORIENTED_EDGE ( 'NONE', *, *, #4449, .T. ) ;
#416 = AXIS2_PLACEMENT_3D ( 'NONE', #4573, #2861, #5177 ) ;
#417 = AXIS2_PLACEMENT_3D ( 'NONE', #6583, #5829, #3680 ) ;
#418 = VERTEX_POINT ( 'NONE', #3343 ) ;
#419 = EDGE_CURVE ( 'NONE', #7087, #6597, #3623, .T. ) ;
#420 = VERTEX_POINT ( 'NONE', #6767 ) ;
#421 = LINE ( 'NONE', #2456, #6291 ) ;
#422 = LINE ( 'NONE', #6729, #6529 ) ;
#423 = FACE_OUTER_BOUND ( 'NONE', #241, .T. ) ;
#424 = AXIS2_PLACEMENT_3D ( 'NONE', #4211, #6401, #703 ) ;
#425 = FACE_OUTER_BOUND ( 'NONE', #7112, .T. ) ;
#426 = CARTESIAN_POINT ( 'NONE',  ( -6.269521507055145548, -62.51903585589134593, 1.741451463471350936 ) ) ;
#427 = VERTEX_POINT ( 'NONE', #5044 ) ;
#428 = CARTESIAN_POINT ( 'NONE',  ( -28.22553731214382111, -35.79092421365019305, -3.001000000000037193 ) ) ;
#429 = EDGE_CURVE ( 'NONE', #3871, #3340, #2130, .T. ) ;
#430 = UNCERTAINTY_MEASURE_WITH_UNIT (LENGTH_MEASURE( 1.000000000000000082E-05 ), #5507, 'distance_accuracy_value', 'NONE');
#431 = DIRECTION ( 'NONE',  ( 5.715354789860003484E-18, 9.999836672264337477E-16, -1.000000000000000000 ) ) ;
#432 = CARTESIAN_POINT ( 'NONE',  ( -1.862703854971429873, -67.54117654042293850, 0.3860096597272351659 ) ) ;
#433 = DIRECTION ( 'NONE',  ( -5.715354789860003484E-18, -9.999836672264337477E-16, 1.000000000000000000 ) ) ;
#434 = EDGE_LOOP ( 'NONE', ( #1898, #6648, #1642, #3197 ) ) ;
#435 = PLANE ( 'NONE',  #6162 ) ;
#436 = CARTESIAN_POINT ( 'NONE',  ( -2.708443266796834781, -56.15294253968003346, -1.503436295530243827 ) ) ;
#437 = DIRECTION ( 'NONE',  ( -0.9999836672264332815, 0.005715354789845002517, 0.000000000000000000 ) ) ;
#438 = CARTESIAN_POINT ( 'NONE',  ( 9.018117650298766108, 16.81805756487467107, -0.3999035282154979054 ) ) ;
#439 = EDGE_CURVE ( 'NONE', #461, #1893, #3908, .T. ) ;
#440 = EDGE_CURVE ( 'NONE', #477, #6355, #744, .T. ) ;
#441 = CARTESIAN_POINT ( 'NONE',  ( 1.159677199572074269, -55.50330010691895666, -1.238196965061255650 ) ) ;
#442 = CARTESIAN_POINT ( 'NONE',  ( -20.47590477366745887, -41.48231850745216320, -3.000000000000042633 ) ) ;
#443 = DIRECTION ( 'NONE',  ( 0.000000000000000000, 0.000000000000000000, 1.000000000000000000 ) ) ;
#444 = B_SPLINE_CURVE_WITH_KNOTS ( 'NONE', 1,
 ( #448, #2731 ),
 .UNSPECIFIED., .F., .F.,
 ( 2, 2 ),
 ( 0.000000000000000000, 1.000000000000000000 ),
 .UNSPECIFIED. ) ;
#445 = EDGE_LOOP ( 'NONE', ( #6799, #6289, #2155, #183 ) ) ;
#446 = ORIENTED_EDGE ( 'NONE', *, *, #1818, .F. ) ;
#447 = DIRECTION ( 'NONE',  ( -0.9999198651055810627, 0.01265951686427546630, 1.265976809860307225E-17 ) ) ;
#448 = CARTESIAN_POINT ( 'NONE',  ( -20.16480223318149356, 14.61937842657788345, -2.993845543551524990 ) ) ;
#449 = ORIENTED_EDGE ( 'NONE', *, *, #4644, .T. ) ;
#450 = CARTESIAN_POINT ( 'NONE',  ( 41.70778007397900211, -94.98992620957551480, 2.999999999999905409 ) ) ;
#451 = EDGE_CURVE ( 'NONE', #5505, #7068, #7351, .T. ) ;
#452 = FACE_OUTER_BOUND ( 'NONE', #2508, .T. ) ;
#453 = LINE ( 'NONE', #485, #6901 ) ;
#454 = CARTESIAN_POINT ( 'NONE',  ( 1.349182120017575981, -67.40498645023109248, 1.310568389067595207 ) ) ;
#455 = DIRECTION ( 'NONE',  ( -0.4328040977884316520, 0.5819352847797604200, 0.6884997728872834788 ) ) ;
#456 = CARTESIAN_POINT ( 'NONE',  ( -109.1076725891878567, -112.1689003517234227, -1.127570259384924611E-13 ) ) ;
#457 = CARTESIAN_POINT ( 'NONE',  ( -18.08304078080998778, 14.25436916875867865, -0.4727591279979656558 ) ) ;
#458 = LINE ( 'NONE', #3308, #1211 ) ;
#459 = CARTESIAN_POINT ( 'NONE',  ( -6.392983792945144295, -62.56006988191466434, 1.848553975009203487 ) ) ;
#460 = ORIENTED_EDGE ( 'NONE', *, *, #4272, .F. ) ;
#461 = VERTEX_POINT ( 'NONE', #5084 ) ;
#462 = CARTESIAN_POINT ( 'NONE',  ( 18.23198843067283548, -39.61652546476334180, 3.399839610809888946 ) ) ;
#463 = DIRECTION ( 'NONE',  ( 0.9986925448795958005, 0.05111947575940636868, 0.000000000000000000 ) ) ;
#464 = LINE ( 'NONE', #4535, #5418 ) ;
#465 = CARTESIAN_POINT ( 'NONE',  ( 6.751207790105429929, -62.61097121624884210, 0.9581327554396804613 ) ) ;
#466 = CARTESIAN_POINT ( 'NONE',  ( 27.55235279947335414, -34.88166451341171381, -3.471129529363089628E-14 ) ) ;
#467 = ORIENTED_EDGE ( 'NONE', *, *, #4073, .T. ) ;
#468 = CARTESIAN_POINT ( 'NONE',  ( -18.51952944085035924, 14.44713361607365876, 0.4060579846639944535 ) ) ;
#469 = ADVANCED_FACE ( 'NONE', ( #5653 ), #6728, .T. ) ;
#470 = CARTESIAN_POINT ( 'NONE',  ( -1.128062821581302000, -55.49617455686423284, 0.7066123397475153611 ) ) ;
#471 = CARTESIAN_POINT ( 'NONE',  ( 18.47982041150265431, -39.47532202006953383, -3.946495907847236140E-14 ) ) ;
#472 = DIRECTION ( 'NONE',  ( -0.9997217333147506713, -0.02358931830619094214, -2.930269742420907704E-17 ) ) ;
#473 = CARTESIAN_POINT ( 'NONE',  ( 1.277257345132870148, -65.35512402512885899, -0.3535023904437397113 ) ) ;
#474 = CARTESIAN_POINT ( 'NONE',  ( 18.06432739836633061, -39.71205113188396041, -3.955074325938771262E-14 ) ) ;
#475 = CARTESIAN_POINT ( 'NONE',  ( 4.746441911065370611, -62.01614811949030326, -2.502481404895003259 ) ) ;
#476 = CARTESIAN_POINT ( 'NONE',  ( -3.427937952159080037, -54.92350006295870202, -2.312565912944844371 ) ) ;
#477 = VERTEX_POINT ( 'NONE', #6809 ) ;
#478 = ORIENTED_EDGE ( 'NONE', *, *, #3847, .T. ) ;
#479 = EDGE_LOOP ( 'NONE', ( #862, #1759, #191, #5380 ) ) ;
#480 = AXIS2_PLACEMENT_3D ( 'NONE', #1466, #4941, #1989 ) ;
#481 = CARTESIAN_POINT ( 'NONE',  ( -105.7473861751082040, -118.0666774205683822, -1.186117176699141851E-13 ) ) ;
#482 = EDGE_LOOP ( 'NONE', ( #4891, #695, #2259, #4148, #2799, #2578 ) ) ;
#483 = FILL_AREA_STYLE_COLOUR ( '', #634 ) ;
#484 = FACE_BOUND ( 'NONE', #3259, .T. ) ;
#485 = CARTESIAN_POINT ( 'NONE',  ( 18.06432739836633061, -39.71205113188396041, 3.999999999999960032 ) ) ;
#486 = CARTESIAN_POINT ( 'NONE',  ( 3.523276076382420019, -54.00647132653568860, -0.5873174244349146367 ) ) ;
#487 = ORIENTED_EDGE ( 'NONE', *, *, #1870, .F. ) ;
#488 = AXIS2_PLACEMENT_3D ( 'NONE', #3919, #348, #4454 ) ;
#489 = VERTEX_POINT ( 'NONE', #4526 ) ;
#490 = EDGE_LOOP ( 'NONE', ( #5569, #3977, #674, #3366 ) ) ;
#491 = EDGE_CURVE ( 'NONE', #4550, #2991, #7293, .T. ) ;
#492 = CARTESIAN_POINT ( 'NONE',  ( -9.311346830843399758, -51.41373841511900622, 2.533728595105000370 ) ) ;
#493 = ADVANCED_FACE ( 'NONE', ( #6254 ), #1091, .T. ) ;
#494 = DIRECTION ( 'NONE',  ( 0.9999836672264335036, -0.005715354789845041548, 0.000000000000000000 ) ) ;
#495 = CARTESIAN_POINT ( 'NONE',  ( -5.206993624623629913, -63.95781028998001716, 3.417603084305509853 ) ) ;
#496 = CIRCLE ( 'NONE', #1095, 2.500000000000000000 ) ;
#497 = DIRECTION ( 'NONE',  ( 0.9147661038495522590, -0.4039838799357101107, 0.000000000000000000 ) ) ;
#498 = DIRECTION ( 'NONE',  ( -0.8795363392562568494, 0.4758317222797389667, 4.707970883985391064E-16 ) ) ;
#499 = CARTESIAN_POINT ( 'NONE',  ( -14.70408710852078116, -35.66654345889202204, -3.575000000000001175E-14 ) ) ;
#500 = CIRCLE ( 'NONE', #2164, 0.9999999999999986677 ) ;
#501 = ORIENTED_EDGE ( 'NONE', *, *, #5222, .F. ) ;
#502 = CARTESIAN_POINT ( 'NONE',  ( 18.74668230531433721, -39.89873697698325117, 3.999999999999960032 ) ) ;
#503 = CARTESIAN_POINT ( 'NONE',  ( -4.748090069711009775, -62.01667038360579198, 2.533819555318849837 ) ) ;
#504 = DIRECTION ( 'NONE',  ( 5.715354789860003484E-18, 9.999836672264337477E-16, -1.000000000000000000 ) ) ;
#505 = CARTESIAN_POINT ( 'NONE',  ( -1.424128410011220147, -67.64226375110297340, -1.734372748508781870 ) ) ;
#506 = CARTESIAN_POINT ( 'NONE',  ( 1.714606436958001585E-17, 2.999951001679301835E-15, -3.000000000000000888 ) ) ;
#507 = VERTEX_POINT ( 'NONE', #2253 ) ;
#508 = ORIENTED_EDGE ( 'NONE', *, *, #1767, .F. ) ;
#509 = CARTESIAN_POINT ( 'NONE',  ( -4.739687333205909958, -61.73825078254577647, 2.268939929871689909 ) ) ;
#510 = CARTESIAN_POINT ( 'NONE',  ( 8.362118858474568484, -51.09933172403994917, -2.502481404895003259 ) ) ;
#511 = LINE ( 'NONE', #5719, #6770 ) ;
#512 = VECTOR ( 'NONE', #1190, 1000.000000000000227 ) ;
#513 = CARTESIAN_POINT ( 'NONE',  ( -5.135436550704829628, -59.04801135763068487, 1.370314102932454814 ) ) ;
#514 = CIRCLE ( 'NONE', #4481, 5.000000000000000000 ) ;
#515 = CARTESIAN_POINT ( 'NONE',  ( 18.38437304540687833, -39.52970360889655410, -0.5000000000000393019 ) ) ;
#516 = CYLINDRICAL_SURFACE ( 'NONE', #4587, 147.0000000000000000 ) ;
#517 = CARTESIAN_POINT ( 'NONE',  ( -5.091256589979570535, -61.80182140578926919, 1.697438579844070761 ) ) ;
#518 = ORIENTED_EDGE ( 'NONE', *, *, #2225, .F. ) ;
#519 = ORIENTED_EDGE ( 'NONE', *, *, #2113, .F. ) ;
#520 = AXIS2_PLACEMENT_3D ( 'NONE', #4684, #6372, #4184 ) ;
#521 = CARTESIAN_POINT ( 'NONE',  ( -12.11759654540111875, 13.15705282150456590, 3.000000000000012879 ) ) ;
#522 = CIRCLE ( 'NONE', #1723, 0.9999999999999998890 ) ;
#523 = CARTESIAN_POINT ( 'NONE',  ( -13.12502771320784056, -36.71825441132875767, 1.026284428608169819 ) ) ;
#524 = DIRECTION ( 'NONE',  ( 5.715354789860003484E-18, 9.999836672264337477E-16, -1.000000000000000000 ) ) ;
#525 = CARTESIAN_POINT ( 'NONE',  ( -7.069128816957480410, -61.66762450778810489, 2.866206824378770168 ) ) ;
#526 = EDGE_CURVE ( 'NONE', #6597, #5379, #1712, .T. ) ;
#527 = AXIS2_PLACEMENT_3D ( 'NONE', #7403, #2247, #4554 ) ;
#528 = AXIS2_PLACEMENT_3D ( 'NONE', #895, #5508, #3787 ) ;
#529 = VECTOR ( 'NONE', #1420, 1000.000000000000000 ) ;
#530 = DIRECTION ( 'NONE',  ( 0.000000000000000000, -1.000000000000000000, -8.673617379884027583E-16 ) ) ;
#531 = DIRECTION ( 'NONE',  ( -0.9999836672264333925, 0.005715354789843017994, -1.984263399433601008E-30 ) ) ;
#532 = CYLINDRICAL_SURFACE ( 'NONE', #864, 1.100000000000000755 ) ;
#533 = LINE ( 'NONE', #2887, #6913 ) ;
#534 = CIRCLE ( 'NONE', #4380, 1.100000000000000755 ) ;
#535 = DIRECTION ( 'NONE',  ( 0.9999836672264332815, -0.005715354789859183882, 0.000000000000000000 ) ) ;
#536 = EDGE_CURVE ( 'NONE', #5972, #2927, #6293, .T. ) ;
#537 = EDGE_CURVE ( 'NONE', #6624, #4598, #3421, .T. ) ;
#538 = ORIENTED_EDGE ( 'NONE', *, *, #4985, .F. ) ;
#539 = TOROIDAL_SURFACE ( 'NONE', #424, 1.500000000000000000, 1.000000000000000000 ) ;
#540 = CARTESIAN_POINT ( 'NONE',  ( 30.36903322412788242, 6.222886872815382553, -1.499999999999994893 ) ) ;
#541 = DIRECTION ( 'NONE',  ( -0.005585937530842041351, -0.9773402531220075629, 0.2116006307393995811 ) ) ;
#542 = EDGE_CURVE ( 'NONE', #1973, #3934, #514, .T. ) ;
#543 = DIRECTION ( 'NONE',  ( -5.715354789860003484E-18, -9.999836672264337477E-16, 1.000000000000000000 ) ) ;
#544 = CARTESIAN_POINT ( 'NONE',  ( 3.523276076382420019, -54.00647132653568860, -0.5873174244349146367 ) ) ;
#545 = CARTESIAN_POINT ( 'NONE',  ( -6.643389330756649613, -62.64438243220202196, 2.533637634891150459 ) ) ;
#546 = ORIENTED_EDGE ( 'NONE', *, *, #3188, .T. ) ;
#547 = CARTESIAN_POINT ( 'NONE',  ( -4.835761215296770388, -62.04624743670729003, 2.958213919140463055 ) ) ;
#548 = CARTESIAN_POINT ( 'NONE',  ( -20.16480223318149356, 14.61937842657788167, 0.006154456448484012937 ) ) ;
#549 = CARTESIAN_POINT ( 'NONE',  ( -32.92087242456759100, 14.53869105662955796, -2.993845543551514776 ) ) ;
#550 = CARTESIAN_POINT ( 'NONE',  ( 4.922451174039159660, -61.67826628571419434, -0.7081498598146799273 ) ) ;
#551 = CARTESIAN_POINT ( 'NONE',  ( 9.998427761233271482, -32.39925913208585939, -3.252606517456513302E-14 ) ) ;
#552 = FACE_OUTER_BOUND ( 'NONE', #4391, .T. ) ;
#553 = VERTEX_POINT ( 'NONE', #7278 ) ;
#554 = ORIENTED_EDGE ( 'NONE', *, *, #3471, .F. ) ;
#555 = VERTEX_POINT ( 'NONE', #5918 ) ;
#556 = B_SPLINE_CURVE_WITH_KNOTS ( 'NONE', 3,
 ( #5245, #2849, #6332, #5736, #1652, #5167, #596, #5949 ),
 .UNSPECIFIED., .F., .F.,
 ( 4, 2, 2, 4 ),
 ( 7.023086426956682172E-18, 0.0003905485738067056029, 0.0007810971476134041585, 0.001562194295226800728 ),
 .UNSPECIFIED. ) ;
#557 = CONTEXT_DEPENDENT_SHAPE_REPRESENTATION ( #3945, #4099 ) ;
#558 = CARTESIAN_POINT ( 'NONE',  ( -33.94153943842304955, 12.25650441806195445, 1.206231629534596424E-14 ) ) ;
#559 = EDGE_LOOP ( 'NONE', ( #876, #3410, #3244, #6024 ) ) ;
#560 = DIRECTION ( 'NONE',  ( -5.715354789845005112E-18, -9.999836672264339449E-16, 1.000000000000000000 ) ) ;
#561 = DIRECTION ( 'NONE',  ( 0.5894575778543340583, -0.6507077505550991070, -0.4786639607048190914 ) ) ;
#562 = CARTESIAN_POINT ( 'NONE',  ( -1.564844514157090138, -53.52797147715784121, 0.2502733031487548443 ) ) ;
#563 = ORIENTED_EDGE ( 'NONE', *, *, #5138, .F. ) ;
#564 = CARTESIAN_POINT ( 'NONE',  ( 15.39900769062488806, 3.181283097128406290, -2.999999999999997335 ) ) ;
#565 = ADVANCED_FACE ( 'NONE', ( #742 ), #2725, .T. ) ;
#566 = DIRECTION ( 'NONE',  ( 0.9999836672264333925, -0.005715354789860572528, 0.000000000000000000 ) ) ;
#567 = CARTESIAN_POINT ( 'NONE',  ( -11.43300101767539623, 1.239551422827354310, 1.301042606982605321E-15 ) ) ;
#568 = DIRECTION ( 'NONE',  ( 5.715354789860003484E-18, 9.999836672264337477E-16, -1.000000000000000000 ) ) ;
#569 = DIRECTION ( 'NONE',  ( 0.9793199139485099236, 0.2023178344681530461, 2.079116908177651401E-16 ) ) ;
#570 = ORIENTED_EDGE ( 'NONE', *, *, #4038, .F. ) ;
#571 = B_SPLINE_CURVE_WITH_KNOTS ( 'NONE', 3,
 ( #1251, #3568, #5855, #6893, #2994, #3601, #5309, #109, #4035, #643 ),
 .UNSPECIFIED., .F., .F.,
 ( 4, 2, 2, 2, 4 ),
 ( 0.000000000000000000, 0.2500000000000000000, 0.5000000000000000000, 0.7500000000000000000, 1.000000000000000000 ),
 .UNSPECIFIED. ) ;
#572 = CARTESIAN_POINT ( 'NONE',  ( -95.86211798318534250, -102.0316339954322018, -1.027823659516258203E-13 ) ) ;
#573 = FACE_OUTER_BOUND ( 'NONE', #2874, .T. ) ;
#574 = CARTESIAN_POINT ( 'NONE',  ( -5.480856739662490540, -62.25220485324549458, 1.560007870815685260 ) ) ;
#575 = CARTESIAN_POINT ( 'NONE',  ( -1.985532163257450078, -53.63691243282757881, -1.870211432998861945 ) ) ;
#576 = CARTESIAN_POINT ( 'NONE',  ( -22.27644891976298780, 9.837844043328869859, 3.306154456448478829 ) ) ;
#577 = VERTEX_POINT ( 'NONE', #442 ) ;
#578 = CARTESIAN_POINT ( 'NONE',  ( -15.07233531785332659, 13.90759097395377886, 2.236547809770392803 ) ) ;
#579 = EDGE_CURVE ( 'NONE', #7422, #1643, #2427, .T. ) ;
#580 = ADVANCED_FACE ( 'NONE', ( #3603 ), #190, .T. ) ;
#581 = DIRECTION ( 'NONE',  ( -5.715354789845005112E-18, -9.999836672264339449E-16, 1.000000000000000000 ) ) ;
#582 = DIRECTION ( 'NONE',  ( -0.7411265327553894222, -0.6713653717953992350, -1.302304562955136501E-15 ) ) ;
#583 = CARTESIAN_POINT ( 'NONE',  ( -2.642495264810874822, -65.73545435749777255, -0.8365618114303696728 ) ) ;
#584 = CARTESIAN_POINT ( 'NONE',  ( 18.49916120972750377, -39.46430250869199341, -0.5000000000000393019 ) ) ;
#585 = CARTESIAN_POINT ( 'NONE',  ( 20.45577244917009097, -23.95683820943715148, -2.383953493077566106E-14 ) ) ;
#586 = ORIENTED_EDGE ( 'NONE', *, *, #2172, .F. ) ;
#587 = ORIENTED_EDGE ( 'NONE', *, *, #4643, .F. ) ;
#588 = EDGE_CURVE ( 'NONE', #6745, #5840, #1526, .T. ) ;
#589 = CARTESIAN_POINT ( 'NONE',  ( -15.08175531864075047, -33.99084820126180517, -5.041145139047909396 ) ) ;
#590 = CARTESIAN_POINT ( 'NONE',  ( 15.01043771185145381, 6.851040774847843906, 6.938893903907228378E-15 ) ) ;
#591 = CARTESIAN_POINT ( 'NONE',  ( -6.240992105565960735, -57.07993508854151798, -2.135104940435555765 ) ) ;
#592 = CARTESIAN_POINT ( 'NONE',  ( 27.24990648202821575, -34.47852395037432416, -0.2518834531394323339 ) ) ;
#593 = CARTESIAN_POINT ( 'NONE',  ( 5.330483863435800274, -59.34891080545844488, 0.6651839376153853012 ) ) ;
#594 = EDGE_LOOP ( 'NONE', ( #6937, #821, #6883, #4560, #734, #2839 ) ) ;
#595 = AXIS2_PLACEMENT_3D ( 'NONE', #4332, #4412, #3266 ) ;
#596 = CARTESIAN_POINT ( 'NONE',  ( 27.99155020439387798, -34.64269665048637137, -0.2641155699549361247 ) ) ;
#597 = DIRECTION ( 'NONE',  ( -0.08966155106958693943, -0.9959722919136836383, 0.000000000000000000 ) ) ;
#598 = DIRECTION ( 'NONE',  ( -0.6713653717954000122, 0.7411265327553888671, 8.673617379884183383E-16 ) ) ;
#599 = AXIS2_PLACEMENT_3D ( 'NONE', #5250, #1318, #2340 ) ;
#600 = DIRECTION ( 'NONE',  ( -5.715354789845005112E-18, -9.999836672264339449E-16, 1.000000000000000000 ) ) ;
#601 = LINE ( 'NONE', #1580, #3108 ) ;
#602 =( NAMED_UNIT ( * ) PLANE_ANGLE_UNIT ( ) SI_UNIT ( $, .RADIAN. ) );
#603 = ORIENTED_EDGE ( 'NONE', *, *, #537, .T. ) ;
#604 = VECTOR ( 'NONE', #6742, 1000.000000000000114 ) ;
#605 = FACE_OUTER_BOUND ( 'NONE', #3752, .T. ) ;
#606 = CARTESIAN_POINT ( 'NONE',  ( 12.08768627091661330, 18.45115358720316223, -2.230393353321891592 ) ) ;
#607 = DIRECTION ( 'NONE',  ( 0.2223191033124283789, 0.6712482523644727195, 0.7071067811865466846 ) ) ;
#608 = CARTESIAN_POINT ( 'NONE',  ( 3.189415849367489564, -54.78201482374456788, -1.959602550130806753 ) ) ;
#609 = EDGE_CURVE ( 'NONE', #3815, #7434, #6716, .T. ) ;
#610 = DIRECTION ( 'NONE',  ( -0.4702355878038426140, 0.002687607115189603359, -0.8825368370389811146 ) ) ;
#611 = EDGE_LOOP ( 'NONE', ( #6371, #3553, #1345 ) ) ;
#612 = CARTESIAN_POINT ( 'NONE',  ( 17.98171507014359349, -40.35658427893240230, 3.523056311642938088 ) ) ;
#613 = FACE_OUTER_BOUND ( 'NONE', #5852, .T. ) ;
#614 = AXIS2_PLACEMENT_3D ( 'NONE', #5442, #1438, #2609 ) ;
#615 = CARTESIAN_POINT ( 'NONE',  ( -43.04083572346265640, -94.50554989113550164, -9.475000000000005065E-14 ) ) ;
#616 = CARTESIAN_POINT ( 'NONE',  ( -14.63712380658832046, -34.60809039433110001, -2.938452842589635683 ) ) ;
#617 = CARTESIAN_POINT ( 'NONE',  ( 5.661089107917369745, -62.15448909529578003, 2.785446686898291002 ) ) ;
#618 = CARTESIAN_POINT ( 'NONE',  ( 27.57050386326208979, -34.29586207421746735, 3.619543086858307390 ) ) ;
#619 = EDGE_CURVE ( 'NONE', #2788, #6597, #2616, .T. ) ;
#620 = CARTESIAN_POINT ( 'NONE',  ( -20.47590477366745887, -41.48231850745216320, -4.159866804656187193E-14 ) ) ;
#621 = EDGE_CURVE ( 'NONE', #138, #7431, #5208, .T. ) ;
#622 = AXIS2_PLACEMENT_3D ( 'NONE', #58, #5292, #6378 ) ;
#623 = ORIENTED_EDGE ( 'NONE', *, *, #2863, .F. ) ;
#624 = ORIENTED_EDGE ( 'NONE', *, *, #5316, .T. ) ;
#625 = ORIENTED_EDGE ( 'NONE', *, *, #588, .F. ) ;
#626 = CARTESIAN_POINT ( 'NONE',  ( 18.11162751801429849, -39.68510166472335499, 3.261603458983328263 ) ) ;
#627 = CIRCLE ( 'NONE', #6512, 5.000000000000000000 ) ;
#628 = AXIS2_PLACEMENT_3D ( 'NONE', #5622, #2168, #455 ) ;
#629 = DIRECTION ( 'NONE',  ( 0.7411265327553895332, 0.6713653717953992350, 1.304512053934558935E-15 ) ) ;
#630 = CARTESIAN_POINT ( 'NONE',  ( 1.773380156858839873, -67.30899524596459571, -0.8098396333890448551 ) ) ;
#631 = CARTESIAN_POINT ( 'NONE',  ( 27.88111011609792556, -34.70420074580282943, -0.5037669066447876265 ) ) ;
#632 = CARTESIAN_POINT ( 'NONE',  ( 2.959376181595404720, -55.87711464508088710, 0.4000749283577051951 ) ) ;
#633 = EDGE_CURVE ( 'NONE', #6064, #2053, #1560, .T. ) ;
#634 = COLOUR_RGB ( '', 0.66274510, 0.83137255, 0.94901961) ;
#635 = ORIENTED_EDGE ( 'NONE', *, *, #339, .F. ) ;
#636 = CIRCLE ( 'NONE', #748, 0.9999999999999984457 ) ;
#637 = TOROIDAL_SURFACE ( 'NONE', #2433, 2.249999999999964917, 1.000000000000000000 ) ;
#638 = DIRECTION ( 'NONE',  ( 0.6713653717953971256, -0.7411265327553914206, -1.022734129183898348E-15 ) ) ;
#639 = CARTESIAN_POINT ( 'NONE',  ( 12.08768627091661330, 18.45115358720316223, -2.230393353321891592 ) ) ;
#640 = AXIS2_PLACEMENT_3D ( 'NONE', #2115, #5499, #7276 ) ;
#641 = DIRECTION ( 'NONE',  ( -0.3213584079436493934, 0.3547505615521249767, -0.8779981849197497912 ) ) ;
#642 = VECTOR ( 'NONE', #2245, 1000.000000000000000 ) ;
#643 = CARTESIAN_POINT ( 'NONE',  ( 5.463696144088109996, -62.30361170774578028, -3.475027489484119769 ) ) ;
#644 = CARTESIAN_POINT ( 'NONE',  ( -5.563801105733269914, -63.69014839564722763, 1.341242183458755344 ) ) ;
#645 = CARTESIAN_POINT ( 'NONE',  ( 14.41492992182968003, -36.00466816619485400, 4.365285548071359045 ) ) ;
#646 = AXIS2_PLACEMENT_3D ( 'NONE', #1626, #5099, #2826 ) ;
#647 = AXIS2_PLACEMENT_3D ( 'NONE', #7275, #6601, #6098 ) ;
#648 = CARTESIAN_POINT ( 'NONE',  ( 2.466033592522905327, -56.00841680802438560, -1.148886392136307943 ) ) ;
#649 = VECTOR ( 'NONE', #1067, 1000.000000000000000 ) ;
#650 = AXIS2_PLACEMENT_3D ( 'NONE', #813, #1935, #1504 ) ;
#651 = CARTESIAN_POINT ( 'NONE',  ( 14.10571919449219891, -36.93826837078879777, -1.990074380419982969 ) ) ;
#652 = CARTESIAN_POINT ( 'NONE',  ( -11.43300101767539623, 1.239551422827354310, 1.301042606982605321E-15 ) ) ;
#653 = CARTESIAN_POINT ( 'NONE',  ( 5.771550998859873438, -61.36048738820532122, 0.6685664931038850511 ) ) ;
#654 = CARTESIAN_POINT ( 'NONE',  ( 1.915558458284230214, -54.23376817553720031, 0.07315972318039029587 ) ) ;
#655 = FACE_OUTER_BOUND ( 'NONE', #1016, .T. ) ;
#656 = AXIS2_PLACEMENT_3D ( 'NONE', #4178, #3567, #4647 ) ;
#657 = ORIENTED_EDGE ( 'NONE', *, *, #1093, .F. ) ;
#658 = CARTESIAN_POINT ( 'NONE',  ( -5.343639688141238686, -62.21333143151184686, 3.460348891136710403 ) ) ;
#659 = EDGE_CURVE ( 'NONE', #3712, #5840, #3389, .T. ) ;
#660 = VECTOR ( 'NONE', #3819, 1000.000000000000000 ) ;
#661 = LINE ( 'NONE', #549, #2800 ) ;
#662 = CARTESIAN_POINT ( 'NONE',  ( 1.919155946380425082, -66.03927477571377835, -1.101811511879709826 ) ) ;
#663 = CARTESIAN_POINT ( 'NONE',  ( -2.887726905928315269, -66.20272978495717098, -0.9560320787877147897 ) ) ;
#664 = CARTESIAN_POINT ( 'NONE',  ( 3.749938752099124972, -0.02143258046197201241, -3.000000000000000888 ) ) ;
#665 = EDGE_LOOP ( 'NONE', ( #2653, #7127, #5002, #3907 ) ) ;
#666 = ORIENTED_EDGE ( 'NONE', *, *, #4440, .T. ) ;
#667 = ORIENTED_EDGE ( 'NONE', *, *, #161, .T. ) ;
#668 = EDGE_CURVE ( 'NONE', #6756, #3571, #1319, .T. ) ;
#669 = EDGE_CURVE ( 'NONE', #3171, #6921, #5083, .T. ) ;
#670 = PLANE ( 'NONE',  #2924 ) ;
#671 = DIRECTION ( 'NONE',  ( 0.9147661038495488173, -0.4039838799357178822, 0.000000000000000000 ) ) ;
#672 = CARTESIAN_POINT ( 'NONE',  ( -3.268733238405740149, -66.73531384189965365, -2.665188268689791862 ) ) ;
#673 = CARTESIAN_POINT ( 'NONE',  ( 18.06432739836606771, -39.71205113188410962, 2.999999999999960476 ) ) ;
#674 = ORIENTED_EDGE ( 'NONE', *, *, #3234, .T. ) ;
#675 = ADVANCED_FACE ( 'NONE', ( #2089 ), #1445, .F. ) ;
#676 = EDGE_CURVE ( 'NONE', #888, #2009, #2043, .T. ) ;
#677 = LINE ( 'NONE', #2816, #3396 ) ;
#678 = CARTESIAN_POINT ( 'NONE',  ( 0.000000000000000000, 0.000000000000000000, 2.544444444444450060 ) ) ;
#679 = DIRECTION ( 'NONE',  ( -0.7411265327553895332, -0.6713653717953993461, -1.302304562955136699E-15 ) ) ;
#680 = DIRECTION ( 'NONE',  ( -0.2023178344681547114, 0.9793199139485095905, 8.673617379884032514E-16 ) ) ;
#681 = CARTESIAN_POINT ( 'NONE',  ( 5.090297305459900556, -61.99464686763499088, 2.430409751936420282 ) ) ;
#682 = DIRECTION ( 'NONE',  ( -0.6713653717954000122, 0.7411265327553888671, 8.673617379884183383E-16 ) ) ;
#683 = CARTESIAN_POINT ( 'NONE',  ( 14.97072768011073940, -34.32654753528365177, 2.597518595105000383 ) ) ;
#684 = LINE ( 'NONE', #6344, #1217 ) ;
#685 = CARTESIAN_POINT ( 'NONE',  ( 6.202282335592980367, -63.50128988325390367, -3.194577187992014622 ) ) ;
#686 = DIRECTION ( 'NONE',  ( 0.9999836672264335036, -0.005715354789845041548, 0.000000000000000000 ) ) ;
#687 = ORIENTED_EDGE ( 'NONE', *, *, #4816, .T. ) ;
#688 = FACE_OUTER_BOUND ( 'NONE', #4920, .T. ) ;
#689 = CARTESIAN_POINT ( 'NONE',  ( 3.749938752099124972, -0.02143258046191576227, 0.000000000000000000 ) ) ;
#690 = CARTESIAN_POINT ( 'NONE',  ( -5.250750166908019878, -57.72135505925717069, -0.3064819419056146188 ) ) ;
#691 = CARTESIAN_POINT ( 'NONE',  ( 1.316624512147740012, -66.75104842734066324, 3.019790780136459851 ) ) ;
#692 = CARTESIAN_POINT ( 'NONE',  ( 14.49911764349215915, -35.75048010860329839, 0.4975185951050001831 ) ) ;
#693 = ORIENTED_EDGE ( 'NONE', *, *, #5607, .F. ) ;
#694 = ADVANCED_FACE ( 'NONE', ( #3779 ), #3812, .F. ) ;
#695 = ORIENTED_EDGE ( 'NONE', *, *, #4767, .T. ) ;
#696 = EDGE_LOOP ( 'NONE', ( #3578, #3253, #1799, #5414 ) ) ;
#697 = FACE_OUTER_BOUND ( 'NONE', #6983, .T. ) ;
#698 = DIRECTION ( 'NONE',  ( -3.872980802086269402E-16, 2.250611045722691657E-16, -1.000000000000000000 ) ) ;
#699 = CARTESIAN_POINT ( 'NONE',  ( -6.321361399357500410, -61.94876894069515316, -0.6341497168666246909 ) ) ;
#700 = DIRECTION ( 'NONE',  ( -5.715354789845005112E-18, -9.999836672264339449E-16, 1.000000000000000000 ) ) ;
#701 = ORIENTED_EDGE ( 'NONE', *, *, #1180, .T. ) ;
#702 = LINE ( 'NONE', #6543, #3867 ) ;
#703 = DIRECTION ( 'NONE',  ( 0.3144019573014849023, -0.9492899500389726519, 0.000000000000000000 ) ) ;
#704 = DIRECTION ( 'NONE',  ( -5.715354789860003484E-18, -9.999836672264337477E-16, 1.000000000000000000 ) ) ;
#705 = CARTESIAN_POINT ( 'NONE',  ( -1.512046953658800152, -54.18079592905042574, 1.959428465566195543 ) ) ;
#706 = ADVANCED_FACE ( 'NONE', ( #360 ), #1383, .T. ) ;
#707 = EDGE_CURVE ( 'NONE', #3483, #3171, #4003, .T. ) ;
#708 = CARTESIAN_POINT ( 'NONE',  ( -2.678905510920184696, -65.04233304593640241, 0.9295552878624004922 ) ) ;
#709 = AXIS2_PLACEMENT_3D ( 'NONE', #6443, #2440, #1841 ) ;
#710 = CARTESIAN_POINT ( 'NONE',  ( -19.14099990134980089, 14.35202449503593058, -2.928563623636439850 ) ) ;
#711 = CARTESIAN_POINT ( 'NONE',  ( 14.49911764349215915, -35.75048010860329839, 0.4975185951050001831 ) ) ;
#712 = CARTESIAN_POINT ( 'NONE',  ( -0.07696283880832878455, -66.23396610719073863, -3.055188877874750020 ) ) ;
#713 = CARTESIAN_POINT ( 'NONE',  ( -5.316774007586650086, -63.89131393482077925, 1.354123676545745170 ) ) ;
#714 = EDGE_CURVE ( 'NONE', #1079, #216, #5791, .T. ) ;
#715 = CIRCLE ( 'NONE', #1687, 1.000000000000000444 ) ;
#716 = VERTEX_POINT ( 'NONE', #1672 ) ;
#717 = DIRECTION ( 'NONE',  ( 5.715354789845005112E-18, 9.999836672264339449E-16, -1.000000000000000000 ) ) ;
#718 = CARTESIAN_POINT ( 'NONE',  ( 39.48483786921892857, -95.33781693134928048, 3.999999999999904521 ) ) ;
#719 = B_SPLINE_CURVE_WITH_KNOTS ( 'NONE', 1,
 ( #5205, #1695 ),
 .UNSPECIFIED., .F., .F.,
 ( 2, 2 ),
 ( 0.000000000000000000, 1.000000000000000000 ),
 .UNSPECIFIED. ) ;
#720 = DIRECTION ( 'NONE',  ( -0.8481698128690331462, 0.5297244269785085224, 5.248681837068071230E-16 ) ) ;
#721 = CARTESIAN_POINT ( 'NONE',  ( 18.11927033577788393, -39.68074713310974744, -0.2519513543403087419 ) ) ;
#722 = UNCERTAINTY_MEASURE_WITH_UNIT (LENGTH_MEASURE( 1.000000000000000082E-05 ), #4037, 'distance_accuracy_value', 'NONE');
#723 = CARTESIAN_POINT ( 'NONE',  ( 1.159215146223531834, -55.24985087088717250, -0.2200125624336850272 ) ) ;
#724 = CARTESIAN_POINT ( 'NONE',  ( -6.708998324124310741, -61.63987295270813860, 3.437611327301279385 ) ) ;
#725 = FACE_OUTER_BOUND ( 'NONE', #7219, .T. ) ;
#726 = ORIENTED_EDGE ( 'NONE', *, *, #2233, .F. ) ;
#727 = ORIENTED_EDGE ( 'NONE', *, *, #7316, .T. ) ;
#728 = ORIENTED_EDGE ( 'NONE', *, *, #5712, .F. ) ;
#729 = PRODUCT ( 'MAS-689', 'MAS-689', '', ( #3217 ) ) ;
#730 = DIRECTION ( 'NONE',  ( 5.715354789860003484E-18, 9.999836672264337477E-16, -1.000000000000000000 ) ) ;
#731 = CARTESIAN_POINT ( 'NONE',  ( 26.87807528571524074, -34.69037653529182563, 2.999999999999965361 ) ) ;
#732 = CARTESIAN_POINT ( 'NONE',  ( -1.855492712959899926, -67.28785520969887557, -0.6321745227666250022 ) ) ;
#733 = CARTESIAN_POINT ( 'NONE',  ( 25.86911032031090940, 23.43408864831972238, -6.178731080732846159 ) ) ;
#734 = ORIENTED_EDGE ( 'NONE', *, *, #3822, .F. ) ;
#735 = EDGE_LOOP ( 'NONE', ( #7209, #6312, #4963, #4617 ) ) ;
#736 = VECTOR ( 'NONE', #1817, 1000.000000000000000 ) ;
#737 = CARTESIAN_POINT ( 'NONE',  ( -14.81339646197689852, -34.80111785677370051, -2.566271404894997499 ) ) ;
#738 = EDGE_CURVE ( 'NONE', #7318, #1826, #636, .T. ) ;
#739 = DIRECTION ( 'NONE',  ( 0.3144066910790611624, 0.9492883822130743221, 0.000000000000000000 ) ) ;
#740 = DIRECTION ( 'NONE',  ( -5.715354789845005112E-18, -9.999836672264339449E-16, 1.000000000000000000 ) ) ;
#741 = LINE ( 'NONE', #1289, #2400 ) ;
#742 = FACE_OUTER_BOUND ( 'NONE', #988, .T. ) ;
#743 = AXIS2_PLACEMENT_3D ( 'NONE', #312, #6591, #3835 ) ;
#744 = CIRCLE ( 'NONE', #628, 1.000000000000000888 ) ;
#745 = CIRCLE ( 'NONE', #1355, 147.0000000000000000 ) ;
#746 = AXIS2_PLACEMENT_3D ( 'NONE', #4808, #7242, #6749 ) ;
#747 = CARTESIAN_POINT ( 'NONE',  ( 1.626596344682255113, -54.75750786503496670, 2.255510009909589719 ) ) ;
#748 = AXIS2_PLACEMENT_3D ( 'NONE', #2153, #1638, #3968 ) ;
#749 = EDGE_CURVE ( 'NONE', #6942, #4841, #1471, .T. ) ;
#750 = EDGE_CURVE ( 'NONE', #6928, #6113, #6639, .T. ) ;
#751 = AXIS2_PLACEMENT_3D ( 'NONE', #5959, #3597, #6467 ) ;
#752 = DIRECTION ( 'NONE',  ( -0.9147661038495488173, 0.4039838799357178822, 0.000000000000000000 ) ) ;
#753 = CARTESIAN_POINT ( 'NONE',  ( -5.431783234843397423, -58.17252153501718226, -0.3016490821137323142 ) ) ;
#754 = CARTESIAN_POINT ( 'NONE',  ( 6.180415987647270626, -62.45112898858806716, 0.6030958204723052551 ) ) ;
#755 = VECTOR ( 'NONE', #3723, 1000.000000000000227 ) ;
#756 = ORIENTED_EDGE ( 'NONE', *, *, #1602, .T. ) ;
#757 = PRODUCT_DEFINITION_FORMATION_WITH_SPECIFIED_SOURCE ( 'ANY', '', #4771, .NOT_KNOWN. ) ;
#758 = CARTESIAN_POINT ( 'NONE',  ( 28.12455780688317475, -37.01391159201033076, 2.999999999999963141 ) ) ;
#759 = AXIS2_PLACEMENT_3D ( 'NONE', #3789, #6111, #1904 ) ;
#760 = VECTOR ( 'NONE', #5141, 1000.000000000000000 ) ;
#761 = EDGE_CURVE ( 'NONE', #6173, #3671, #7429, .T. ) ;
#762 = CARTESIAN_POINT ( 'NONE',  ( -95.86211798318534250, -102.0316339954322018, 3.999999999999897859 ) ) ;
#763 = CARTESIAN_POINT ( 'NONE',  ( 17.88843813772660596, -40.41242482300715011, -0.1308508315819079393 ) ) ;
#764 = CARTESIAN_POINT ( 'NONE',  ( -6.097705871868670080, -61.85866295707492668, 3.539665806518350610 ) ) ;
#765 = CIRCLE ( 'NONE', #6539, 0.5000000000000004441 ) ;
#766 = CARTESIAN_POINT ( 'NONE',  ( -2.527830428429834964, -65.26309079616396502, -2.780623214462280668 ) ) ;
#767 = AXIS2_PLACEMENT_3D ( 'NONE', #871, #3769, #5908 ) ;
#768 = CARTESIAN_POINT ( 'NONE',  ( -6.129265975028279634, -62.42766041111902098, -0.6909925287373350766 ) ) ;
#769 = LINE ( 'NONE', #2532, #132 ) ;
#770 = ORIENTED_EDGE ( 'NONE', *, *, #978, .T. ) ;
#771 = EDGE_LOOP ( 'NONE', ( #5192, #1574, #5528, #7020, #5156 ) ) ;
#772 = ORIENTED_EDGE ( 'NONE', *, *, #2683, .F. ) ;
#773 = ORIENTED_EDGE ( 'NONE', *, *, #2365, .T. ) ;
#774 = AXIS2_PLACEMENT_3D ( 'NONE', #1957, #4270, #4224 ) ;
#775 = CARTESIAN_POINT ( 'NONE',  ( -13.14279338728291080, 13.42477640308646514, 3.000000000000013323 ) ) ;
#776 = FACE_OUTER_BOUND ( 'NONE', #2120, .T. ) ;
#777 = CARTESIAN_POINT ( 'NONE',  ( 5.248671903609490208, -63.99330799355751509, -3.505550301244489741 ) ) ;
#778 = ORIENTED_EDGE ( 'NONE', *, *, #5101, .T. ) ;
#779 = EDGE_LOOP ( 'NONE', ( #7399, #930, #4175, #7407 ) ) ;
#780 = DIRECTION ( 'NONE',  ( 0.2164621326156030423, -0.07169280077033016174, 0.9736551173085935540 ) ) ;
#781 = DIRECTION ( 'NONE',  ( 0.9999836672264332815, -0.005715354789859183882, 0.000000000000000000 ) ) ;
#782 = DIRECTION ( 'NONE',  ( 0.9793199139485104787, 0.2023178344681509366, 2.079116908177630447E-16 ) ) ;
#783 = CARTESIAN_POINT ( 'NONE',  ( -6.097705871868670080, -61.85866295707492668, 3.539665806518350610 ) ) ;
#784 = ORIENTED_EDGE ( 'NONE', *, *, #6468, .F. ) ;
#785 = EDGE_LOOP ( 'NONE', ( #5644, #3488, #7009, #2675, #2047, #4651 ) ) ;
#786 = EDGE_CURVE ( 'NONE', #5766, #1922, #4465, .T. ) ;
#787 = CARTESIAN_POINT ( 'NONE',  ( -10.54744521951312208, -8.271218886098248291, -8.331366185709195643E-15 ) ) ;
#788 = CARTESIAN_POINT ( 'NONE',  ( 4.977719985769329725, -63.63849604921595216, 2.874328699340139792 ) ) ;
#789 = CARTESIAN_POINT ( 'NONE',  ( 9.311407240687648468, -51.41373841511902043, -1.002481404894999928 ) ) ;
#790 = CARTESIAN_POINT ( 'NONE',  ( -32.59768532061891477, 15.27050393970957565, -0.7438455435515303193 ) ) ;
#791 = CARTESIAN_POINT ( 'NONE',  ( 4.372548960228861858, -64.23807538291029573, -1.245661913065559734 ) ) ;
#792 = ORIENTED_EDGE ( 'NONE', *, *, #6202, .T. ) ;
#793 = ADVANCED_FACE ( 'NONE', ( #5721 ), #6794, .F. ) ;
#794 = FACE_OUTER_BOUND ( 'NONE', #2300, .T. ) ;
#795 = CYLINDRICAL_SURFACE ( 'NONE', #5962, 20.00000000000000711 ) ;
#796 = CARTESIAN_POINT ( 'NONE',  ( 3.749938752099124972, -0.02143258046191576227, 0.000000000000000000 ) ) ;
#797 = UNCERTAINTY_MEASURE_WITH_UNIT (LENGTH_MEASURE( 1.000000000000000082E-05 ), #6381, 'distance_accuracy_value', 'NONE');
#798 = CARTESIAN_POINT ( 'NONE',  ( 5.661113010068490325, -57.37064013373739613, 2.401523511004880262 ) ) ;
#799 = FACE_OUTER_BOUND ( 'NONE', #1045, .T. ) ;
#800 = DIRECTION ( 'NONE',  ( -0.9147661038495522590, 0.4039838799357101107, 0.000000000000000000 ) ) ;
#801 = ORIENTED_EDGE ( 'NONE', *, *, #2322, .T. ) ;
#802 = EDGE_CURVE ( 'NONE', #7250, #6854, #6673, .T. ) ;
#803 = EDGE_CURVE ( 'NONE', #5496, #7250, #1244, .T. ) ;
#804 = ORIENTED_EDGE ( 'NONE', *, *, #971, .F. ) ;
#805 = CARTESIAN_POINT ( 'NONE',  ( 9.358334193258830425, -51.27205182843857045, -2.495037190209991707 ) ) ;
#806 = DIRECTION ( 'NONE',  ( -0.3144066910790599412, -0.9492883822130747662, 0.000000000000000000 ) ) ;
#807 = CARTESIAN_POINT ( 'NONE',  ( 2.440761905804889942, -65.30842328614467363, 1.105894752426585415 ) ) ;
#808 = CARTESIAN_POINT ( 'NONE',  ( -5.904042796847299712, -62.42803713013675093, 3.506543003539000392 ) ) ;
#809 = EDGE_LOOP ( 'NONE', ( #5426, #6635, #3694, #2758 ) ) ;
#810 = ORIENTED_EDGE ( 'NONE', *, *, #2697, .F. ) ;
#811 = DIRECTION ( 'NONE',  ( 5.715354789845005112E-18, 9.999836672264339449E-16, -1.000000000000000000 ) ) ;
#812 = CARTESIAN_POINT ( 'NONE',  ( 3.888488774788935842, 0.9378992740910084835, -17.67054229618195293 ) ) ;
#813 = CARTESIAN_POINT ( 'NONE',  ( -16.17971834312690760, 1.679495322419672920, 0.9550319896483219217 ) ) ;
#814 = ORIENTED_EDGE ( 'NONE', *, *, #429, .F. ) ;
#815 = VERTEX_POINT ( 'NONE', #2271 ) ;
#816 = DIRECTION ( 'NONE',  ( -5.715354789845005112E-18, -9.999836672264339449E-16, 1.000000000000000000 ) ) ;
#817 = CARTESIAN_POINT ( 'NONE',  ( -0.9970853242166300978, -65.67144495878099519, -1.280490079922569802 ) ) ;
#818 = CARTESIAN_POINT ( 'NONE',  ( 27.11783474234813340, -35.12923323413248511, 3.499999999999964917 ) ) ;
#819 = DIRECTION ( 'NONE',  ( -0.9999836672264335036, 0.005715354789845008589, 0.000000000000000000 ) ) ;
#820 = CARTESIAN_POINT ( 'NONE',  ( 4.754243898017194603, -57.04914850836969009, -1.691473023288849742 ) ) ;
#821 = ORIENTED_EDGE ( 'NONE', *, *, #4240, .T. ) ;
#822 = CYLINDRICAL_SURFACE ( 'NONE', #4723, 147.0000000000000284 ) ;
#823 = VECTOR ( 'NONE', #7264, 1000.000000000000114 ) ;
#824 = CYLINDRICAL_SURFACE ( 'NONE', #5814, 2.249999999999962252 ) ;
#825 = DIRECTION ( 'NONE',  ( 0.1860016876085203719, -0.1636620475539280195, 0.9688230521603200529 ) ) ;
#826 = LINE ( 'NONE', #796, #7371 ) ;
#827 = EDGE_CURVE ( 'NONE', #7060, #7093, #4582, .T. ) ;
#828 = CARTESIAN_POINT ( 'NONE',  ( -1.974098099753330171, -66.57628266072889289, 3.196874607719439876 ) ) ;
#829 = CARTESIAN_POINT ( 'NONE',  ( -3.508682979600159957, -66.46637211483655960, 1.044995729122755179 ) ) ;
#830 = PLANE ( 'NONE',  #614 ) ;
#831 = ORIENTED_EDGE ( 'NONE', *, *, #4632, .T. ) ;
#832 = ORIENTED_EDGE ( 'NONE', *, *, #4592, .F. ) ;
#833 = AXIS2_PLACEMENT_3D ( 'NONE', #2348, #5745, #4043 ) ;
#834 = CARTESIAN_POINT ( 'NONE',  ( 9.311407240687648468, -51.41373841511902043, -3.502481404894999706 ) ) ;
#835 = CARTESIAN_POINT ( 'NONE',  ( 1.172374092613760688, -4.860610968486169803, 3.500000000000000000 ) ) ;
#836 = EDGE_CURVE ( 'NONE', #6064, #5997, #4487, .T. ) ;
#837 = EDGE_CURVE ( 'NONE', #716, #1124, #6410, .T. ) ;
#838 = CARTESIAN_POINT ( 'NONE',  ( 5.253257825778660184, -59.02147093648149223, -1.455491405082765866 ) ) ;
#839 = CARTESIAN_POINT ( 'NONE',  ( 6.214916356356757099, -59.39665835591213749, 2.509282487442340948 ) ) ;
#840 = AXIS2_PLACEMENT_3D ( 'NONE', #4513, #4429, #7314 ) ;
#841 = EDGE_LOOP ( 'NONE', ( #6668, #2509, #3147, #2037 ) ) ;
#842 = ORIENTED_EDGE ( 'NONE', *, *, #1448, .F. ) ;
#843 = ORIENTED_EDGE ( 'NONE', *, *, #5006, .F. ) ;
#844 = CARTESIAN_POINT ( 'NONE',  ( 0.000000000000000000, 0.000000000000000000, 0.000000000000000000 ) ) ;
#845 = DIRECTION ( 'NONE',  ( 5.715354789845005112E-18, 9.999836672264339449E-16, -1.000000000000000000 ) ) ;
#846 = PRODUCT ( 'Pliers Left Handle Arm', 'Pliers Left Handle Arm', '', ( #5727 ) ) ;
#847 = ADVANCED_FACE ( 'NONE', ( #7018 ), #4192, .T. ) ;
#848 = CARTESIAN_POINT ( 'NONE',  ( 39.48483786921892857, -95.33781693134928048, 2.999999999999904965 ) ) ;
#849 = CARTESIAN_POINT ( 'NONE',  ( -16.51707533432788111, -40.85914143033993895, -3.000000000000041744 ) ) ;
#850 = CARTESIAN_POINT ( 'NONE',  ( 3.592758869166885471, -66.41582265024271692, 0.6922273147611399668 ) ) ;
#851 = ORIENTED_EDGE ( 'NONE', *, *, #4724, .T. ) ;
#852 = ORIENTED_EDGE ( 'NONE', *, *, #5139, .T. ) ;
#853 = EDGE_LOOP ( 'NONE', ( #2489, #4961 ) ) ;
#854 = CARTESIAN_POINT ( 'NONE',  ( 14.63724902514210058, -36.05867701049984930, 4.346656902870709160 ) ) ;
#855 = CARTESIAN_POINT ( 'NONE',  ( 5.175864525269250116, -61.68163375030346174, 0.3100344153189201202 ) ) ;
#856 = DIRECTION ( 'NONE',  ( 0.4644123028815776988, -0.8856191127862077517, -8.829503670900357056E-16 ) ) ;
#857 = VECTOR ( 'NONE', #5182, 1000.000000000000227 ) ;
#858 = EDGE_CURVE ( 'NONE', #4757, #5242, #6486, .T. ) ;
#859 = VECTOR ( 'NONE', #2007, 1000.000000000000000 ) ;
#860 = LINE ( 'NONE', #4298, #4326 ) ;
#861 = CARTESIAN_POINT ( 'NONE',  ( -3.816438721764812136, -64.79865757078124489, -2.819062171272241901 ) ) ;
#862 = ORIENTED_EDGE ( 'NONE', *, *, #1392, .T. ) ;
#863 = STYLED_ITEM ( 'NONE', ( #5858 ), #2394 ) ;
#864 = AXIS2_PLACEMENT_3D ( 'NONE', #2929, #2850, #6848 ) ;
#865 = AXIS2_PLACEMENT_3D ( 'NONE', #7223, #2593, #904 ) ;
#866 = CARTESIAN_POINT ( 'NONE',  ( -14.49899450467539985, -35.75040780681265318, -2.566271404894997499 ) ) ;
#867 = LINE ( 'NONE', #3121, #7137 ) ;
#868 = CARTESIAN_POINT ( 'NONE',  ( -12.80424950550273167, -30.40040925781620373, -3.000000000000031086 ) ) ;
#869 = TOROIDAL_SURFACE ( 'NONE', #275, 147.0000000000000000, 1.000000000000000000 ) ;
#870 = CARTESIAN_POINT ( 'NONE',  ( -5.628700163094269016, -63.23550210468251009, 3.461537593744290042 ) ) ;
#871 = CARTESIAN_POINT ( 'NONE',  ( 27.55235279947361349, -34.88166451341158592, 3.999999999999965361 ) ) ;
#872 = CIRCLE ( 'NONE', #1358, 2.999999999999999556 ) ;
#873 = CARTESIAN_POINT ( 'NONE',  ( 6.131131505788760094, -57.13037711201883440, 2.282642250695309905 ) ) ;
#874 = CARTESIAN_POINT ( 'NONE',  ( -28.98392423323637601, 11.10561281704045200, -1.499999999999989564 ) ) ;
#875 = CIRCLE ( 'NONE', #4505, 1.100000000000000755 ) ;
#876 = ORIENTED_EDGE ( 'NONE', *, *, #1819, .T. ) ;
#877 = ORIENTED_EDGE ( 'NONE', *, *, #633, .F. ) ;
#878 = VERTEX_POINT ( 'NONE', #1889 ) ;
#879 = ADVANCED_FACE ( 'NONE', ( #799 ), #2886, .T. ) ;
#880 = AXIS2_PLACEMENT_3D ( 'NONE', #4624, #4579, #3475 ) ;
#881 = FACE_BOUND ( 'NONE', #4518, .T. ) ;
#882 = CIRCLE ( 'NONE', #5955, 147.0000000000000000 ) ;
#883 = AXIS2_PLACEMENT_3D ( 'NONE', #1572, #1012, #5541 ) ;
#884 = CARTESIAN_POINT ( 'NONE',  ( 17.88843813672055916, -40.41242482140537362, 3.999999999999959144 ) ) ;
#885 = CARTESIAN_POINT ( 'NONE',  ( 4.826828241146579934, -57.92957641372471755, 0.5758163846279100717 ) ) ;
#886 = DIRECTION ( 'NONE',  ( 0.6713653717953965705, -0.7411265327553918647, -7.095217611944926095E-16 ) ) ;
#887 = CARTESIAN_POINT ( 'NONE',  ( -5.586110484983932700, -63.35381962756557783, 1.355548068171432252 ) ) ;
#888 = VERTEX_POINT ( 'NONE', #5085 ) ;
#889 = AXIS2_PLACEMENT_3D ( 'NONE', #6367, #5354, #2966 ) ;
#890 = ORIENTED_EDGE ( 'NONE', *, *, #5, .F. ) ;
#891 = EDGE_LOOP ( 'NONE', ( #5274, #7034, #3632, #1068 ) ) ;
#892 = EDGE_CURVE ( 'NONE', #5232, #3517, #2314, .T. ) ;
#893 = ADVANCED_FACE ( 'NONE', ( #423 ), #3307, .T. ) ;
#894 = DIRECTION ( 'NONE',  ( 0.000000000000000000, 0.000000000000000000, 1.000000000000000000 ) ) ;
#895 = CARTESIAN_POINT ( 'NONE',  ( -17.18648583462957902, 1.679248046991888677, -3.299999999999998046 ) ) ;
#896 = DIRECTION ( 'NONE',  ( 5.715354789845005112E-18, 9.999836672264339449E-16, -1.000000000000000000 ) ) ;
#897 = CARTESIAN_POINT ( 'NONE',  ( -32.93157973858376408, 14.54341967768581512, 1.435496648130876646E-14 ) ) ;
#898 = CARTESIAN_POINT ( 'NONE',  ( 5.267626090836840191, -63.86700364562991439, -1.442031773567929775 ) ) ;
#899 = ORIENTED_EDGE ( 'NONE', *, *, #5637, .F. ) ;
#900 = ORIENTED_EDGE ( 'NONE', *, *, #1718, .F. ) ;
#901 = VERTEX_POINT ( 'NONE', #4675 ) ;
#902 = ADVANCED_FACE ( 'NONE', ( #5809 ), #5168, .T. ) ;
#903 = ADVANCED_FACE ( 'NONE', ( #1173 ), #6519, .T. ) ;
#904 = DIRECTION ( 'NONE',  ( -0.2163384215910431896, -0.07165063022625259292, 0.9736857165079894072 ) ) ;
#905 = CARTESIAN_POINT ( 'NONE',  ( -3.569041007005829602, -65.81017109676685095, 3.284668648760890264 ) ) ;
#906 = ORIENTED_EDGE ( 'NONE', *, *, #7286, .F. ) ;
#907 = CARTESIAN_POINT ( 'NONE',  ( -6.643389330756649613, -62.64438243220202196, 2.533637634891150459 ) ) ;
#908 = LINE ( 'NONE', #3797, #4212 ) ;
#909 = VERTEX_POINT ( 'NONE', #6889 ) ;
#910 = EDGE_CURVE ( 'NONE', #3970, #2280, #5227, .T. ) ;
#911 = FACE_OUTER_BOUND ( 'NONE', #4195, .T. ) ;
#912 = FACE_OUTER_BOUND ( 'NONE', #841, .T. ) ;
#913 = FACE_OUTER_BOUND ( 'NONE', #3093, .T. ) ;
#914 = CARTESIAN_POINT ( 'NONE',  ( 5.416018991692120643, -63.93240027730202968, 2.754852738177090643 ) ) ;
#915 = CARTESIAN_POINT ( 'NONE',  ( 6.647873823884112632, -62.63640551056316497, -2.279271695592409497 ) ) ;
#916 = CARTESIAN_POINT ( 'NONE',  ( 6.663059173928499668, -62.48704134639812935, 2.547684199221960100 ) ) ;
#917 = CARTESIAN_POINT ( 'NONE',  ( -34.88460058024264043, 16.28046363954882736, -1.493845543551999944 ) ) ;
#918 = EDGE_LOOP ( 'NONE', ( #5155, #6456, #1274, #4233 ) ) ;
#919 = LINE ( 'NONE', #1633, #2892 ) ;
#920 = ORIENTED_EDGE ( 'NONE', *, *, #714, .T. ) ;
#921 = DIRECTION ( 'NONE',  ( 0.9793199139485103677, 0.2023178344681514362, 2.079116908177635377E-16 ) ) ;
#922 = CARTESIAN_POINT ( 'NONE',  ( 35.25551690214635414, 7.283442040853450372, -2.999999999999993339 ) ) ;
#923 = CARTESIAN_POINT ( 'NONE',  ( 4.756074659365879143, -62.80135681555328375, -3.311393743080873975 ) ) ;
#924 = CARTESIAN_POINT ( 'NONE',  ( 1.714606436953501688E-17, 2.999951001679301835E-15, 0.000000000000000000 ) ) ;
#925 = ORIENTED_CLOSED_SHELL ( 'NONE', *, #3017, .F. );
#926 = CARTESIAN_POINT ( 'NONE',  ( -5.894573565049844532, -58.07158296836707478, 1.644009501509583027 ) ) ;
#927 = ORIENTED_EDGE ( 'NONE', *, *, #5460, .F. ) ;
#928 = ORIENTED_EDGE ( 'NONE', *, *, #659, .F. ) ;
#929 = EDGE_LOOP ( 'NONE', ( #2961, #1882, #6390, #623 ) ) ;
#930 = ORIENTED_EDGE ( 'NONE', *, *, #6257, .T. ) ;
#931 = CARTESIAN_POINT ( 'NONE',  ( -17.21006346072928750, 13.86884027412869180, -2.230393353321906247 ) ) ;
#932 = DIRECTION ( 'NONE',  ( 5.715354789845005112E-18, 9.999836672264339449E-16, -1.000000000000000000 ) ) ;
#933 = FACE_OUTER_BOUND ( 'NONE', #1417, .T. ) ;
#934 = CARTESIAN_POINT ( 'NONE',  ( -1.206827191127304078, -66.77204028133226643, -1.044217440639481742 ) ) ;
#935 = EDGE_CURVE ( 'NONE', #2431, #6755, #5853, .T. ) ;
#936 = VERTEX_POINT ( 'NONE', #107 ) ;
#937 = VERTEX_POINT ( 'NONE', #5247 ) ;
#938 = ORIENTED_EDGE ( 'NONE', *, *, #6081, .T. ) ;
#939 = LINE ( 'NONE', #456, #5214 ) ;
#940 = CARTESIAN_POINT ( 'NONE',  ( -1.095027572700850049, -66.25608112803911354, -0.9253912358714898589 ) ) ;
#941 = DIRECTION ( 'NONE',  ( 5.715354789845005112E-18, 9.999836672264339449E-16, -1.000000000000000000 ) ) ;
#942 = EDGE_CURVE ( 'NONE', #3934, #6950, #6758, .T. ) ;
#943 = EDGE_CURVE ( 'NONE', #2698, #3646, #2185, .T. ) ;
#944 = CARTESIAN_POINT ( 'NONE',  ( -5.667613743078470101, -62.32074054030601928, 1.527775587545428193 ) ) ;
#945 = EDGE_LOOP ( 'NONE', ( #1825, #3595, #603, #5681 ) ) ;
#946 = CARTESIAN_POINT ( 'NONE',  ( 9.358334193258830425, -51.27205182843857045, -2.495037190209989930 ) ) ;
#947 = FACE_OUTER_BOUND ( 'NONE', #2701, .T. ) ;
#948 = CARTESIAN_POINT ( 'NONE',  ( 6.319659661046010513, -62.49917928162491876, -1.706589513406323366 ) ) ;
#949 = CARTESIAN_POINT ( 'NONE',  ( -1.678659834933539985, -53.30027862203323252, 1.268182062803870247 ) ) ;
#950 = DIRECTION ( 'NONE',  ( -0.4039838799357112764, -0.9147661038495517039, -1.194615830541411051E-15 ) ) ;
#951 = AXIS2_PLACEMENT_3D ( 'NONE', #2596, #2632, #3683 ) ;
#952 = EDGE_LOOP ( 'NONE', ( #1384, #5365, #5929, #3739 ) ) ;
#953 = DIRECTION ( 'NONE',  ( -5.715354789845005112E-18, -9.999836672264339449E-16, 1.000000000000000000 ) ) ;
#954 = CARTESIAN_POINT ( 'NONE',  ( 13.49911764349216092, -35.75048010860329839, 0.4975185951050001831 ) ) ;
#955 = AXIS2_PLACEMENT_3D ( 'NONE', #1918, #6091, #7082 ) ;
#956 = LINE ( 'NONE', #4314, #4970 ) ;
#957 = CARTESIAN_POINT ( 'NONE',  ( -4.248468832057555211, -63.21868707083201855, -2.033638508047526550 ) ) ;
#958 = CARTESIAN_POINT ( 'NONE',  ( 27.99155020439384955, -34.64269665048638558, 2.999999999999965361 ) ) ;
#959 = CARTESIAN_POINT ( 'NONE',  ( 6.164870568366772829, -59.43741054342344654, 0.4113734782956702252 ) ) ;
#960 = ORIENTED_EDGE ( 'NONE', *, *, #5662, .F. ) ;
#961 = VERTEX_POINT ( 'NONE', #2965 ) ;
#962 = ORIENTED_EDGE ( 'NONE', *, *, #1280, .T. ) ;
#963 = COLOUR_RGB ( '', 0.31764706, 0.68627451, 0.89019608) ;
#964 = PRODUCT_CONTEXT ( 'NONE', #2544, 'mechanical' ) ;
#965 = DIRECTION ( 'NONE',  ( 0.9999836672264332815, -0.005715354789859975783, 0.000000000000000000 ) ) ;
#966 = FACE_OUTER_BOUND ( 'NONE', #5767, .T. ) ;
#967 = VECTOR ( 'NONE', #2871, 999.9999999999998863 ) ;
#968 = FACE_OUTER_BOUND ( 'NONE', #3719, .T. ) ;
#969 = CARTESIAN_POINT ( 'NONE',  ( -6.490403473174280791, -62.28500686936251185, 3.403714661497959870 ) ) ;
#970 = DIRECTION ( 'NONE',  ( -5.715354789860003484E-18, -9.999836672264337477E-16, 1.000000000000000000 ) ) ;
#971 = EDGE_CURVE ( 'NONE', #7093, #6135, #4708, .T. ) ;
#972 = DIRECTION ( 'NONE',  ( 0.1845982795403117716, 0.9828140593167952188, 9.838530518984746718E-16 ) ) ;
#973 = CARTESIAN_POINT ( 'NONE',  ( 6.285636693253979779, -59.03245517747429716, 2.489777307435960374 ) ) ;
#974 = CARTESIAN_POINT ( 'NONE',  ( 20.45577244917009097, -23.95683820943714792, -3.000000000000024869 ) ) ;
#975 = LINE ( 'NONE', #7225, #5548 ) ;
#976 = AXIS2_PLACEMENT_3D ( 'NONE', #3320, #6787, #3923 ) ;
#977 = ORIENTED_EDGE ( 'NONE', *, *, #5252, .T. ) ;
#978 = EDGE_CURVE ( 'NONE', #3496, #75, #3836, .T. ) ;
#979 = EDGE_CURVE ( 'NONE', #3069, #4278, #4033, .T. ) ;
#980 = AXIS2_PLACEMENT_3D ( 'NONE', #2792, #4661, #4049 ) ;
#981 = VECTOR ( 'NONE', #886, 1000.000000000000114 ) ;
#982 = LINE ( 'NONE', #1590, #1137 ) ;
#983 = DIRECTION ( 'NONE',  ( -0.9492899500389727629, -0.3144019573014849023, 0.000000000000000000 ) ) ;
#984 = CARTESIAN_POINT ( 'NONE',  ( 1.349182120017575981, -67.40498645023109248, 1.310568389067595207 ) ) ;
#985 = DIRECTION ( 'NONE',  ( 0.1860016876085203441, -0.1636620475539279917, 0.9688230521603200529 ) ) ;
#986 = CIRCLE ( 'NONE', #390, 0.9999999999999998890 ) ;
#987 = AXIS2_PLACEMENT_3D ( 'NONE', #3584, #3663, #4763 ) ;
#988 = EDGE_LOOP ( 'NONE', ( #727, #6330, #1513, #4803 ) ) ;
#989 =( GEOMETRIC_REPRESENTATION_CONTEXT ( 3 ) GLOBAL_UNCERTAINTY_ASSIGNED_CONTEXT ( ( #274 ) ) GLOBAL_UNIT_ASSIGNED_CONTEXT ( ( #185, #5991, #3638 ) ) REPRESENTATION_CONTEXT ( 'NONE', 'WORKASPACE' ) );
#990 = FACE_OUTER_BOUND ( 'NONE', #1162, .T. ) ;
#991 = ADVANCED_FACE ( 'NONE', ( #5202 ), #532, .F. ) ;
#992 = DIRECTION ( 'NONE',  ( 5.715354789860003484E-18, 9.999836672264337477E-16, -1.000000000000000000 ) ) ;
#993 = CIRCLE ( 'NONE', #6523, 2.500000000000000000 ) ;
#994 = VECTOR ( 'NONE', #5299, 1000.000000000000114 ) ;
#995 = DIRECTION ( 'NONE',  ( 0.3144066910790613845, 0.9492883822130742111, 0.000000000000000000 ) ) ;
#996 = CARTESIAN_POINT ( 'NONE',  ( -1.630661209647960019, -65.50972637651682362, 2.960670344429949807 ) ) ;
#997 = AXIS2_PLACEMENT_3D ( 'NONE', #3817, #7254, #447 ) ;
#998 = DIRECTION ( 'NONE',  ( 0.9999836672264333925, -0.005715354789844388425, 0.000000000000000000 ) ) ;
#999 = CARTESIAN_POINT ( 'NONE',  ( -4.429163702585058537, -56.03682623248362660, -0.3226722266289872576 ) ) ;
#1000 = VERTEX_POINT ( 'NONE', #6366 ) ;
#1001 = CARTESIAN_POINT ( 'NONE',  ( 5.674632694949170109, -63.26545500802649258, -3.549449971387770297 ) ) ;
#1002 = ORIENTED_EDGE ( 'NONE', *, *, #7088, .T. ) ;
#1003 = AXIS2_PLACEMENT_3D ( 'NONE', #6627, #2572, #347 ) ;
#1004 = ORIENTED_EDGE ( 'NONE', *, *, #7088, .F. ) ;
#1005 = VERTEX_POINT ( 'NONE', #3490 ) ;
#1006 = CIRCLE ( 'NONE', #647, 147.0000000000000000 ) ;
#1007 = AXIS2_PLACEMENT_3D ( 'NONE', #5614, #4434, #4286 ) ;
#1008 = AXIS2_PLACEMENT_3D ( 'NONE', #6368, #1212, #704 ) ;
#1009 = DIRECTION ( 'NONE',  ( 0.000000000000000000, 0.000000000000000000, 1.000000000000000000 ) ) ;
#1010 = DIRECTION ( 'NONE',  ( 0.3144066910790610514, 0.9492883822130744331, 0.000000000000000000 ) ) ;
#1011 = DIRECTION ( 'NONE',  ( -0.005715354789845003385, -0.9999836672264335036, -1.000000000000000472E-15 ) ) ;
#1012 = DIRECTION ( 'NONE',  ( 0.4094857180573137634, -0.9123165276958903336, -9.099612708765444388E-16 ) ) ;
#1013 = CARTESIAN_POINT ( 'NONE',  ( -6.126235009943979293, -64.48141016635396738, -1.469515951087519978 ) ) ;
#1014 = EDGE_LOOP ( 'NONE', ( #403, #1276, #2986, #6808 ) ) ;
#1015 = CIRCLE ( 'NONE', #3763, 147.0000000000000000 ) ;
#1016 = EDGE_LOOP ( 'NONE', ( #4893, #6389, #4139 ) ) ;
#1017 = CARTESIAN_POINT ( 'NONE',  ( -17.04733905648494030, -8.234069079964159599, -8.331366185709195643E-15 ) ) ;
#1018 = DIRECTION ( 'NONE',  ( 0.3144019573014853464, -0.9492899500389726519, -7.355227538141627568E-16 ) ) ;
#1019 = CARTESIAN_POINT ( 'NONE',  ( 5.929218414971320072, -62.35084102844776055, -1.530333388185332932 ) ) ;
#1020 = VECTOR ( 'NONE', #3459, 1000.000000000000000 ) ;
#1021 = CARTESIAN_POINT ( 'NONE',  ( 27.88123484459569568, -34.70413128614676168, 3.503735202131379900 ) ) ;
#1022 = DIRECTION ( 'NONE',  ( -0.9999836672264332815, 0.005715354789859956701, 0.000000000000000000 ) ) ;
#1023 = EDGE_CURVE ( 'NONE', #5766, #716, #1835, .T. ) ;
#1024 = ORIENTED_EDGE ( 'NONE', *, *, #261, .T. ) ;
#1025 = B_SPLINE_CURVE_WITH_KNOTS ( 'NONE', 3,
 ( #4575, #3398, #2302, #91, #1665, #612, #4005, #4077 ),
 .UNSPECIFIED., .F., .F.,
 ( 4, 2, 2, 4 ),
 ( 0.000000000000000000, 0.0003905813100143790020, 0.0007811626200287574619, 0.001562325240057513189 ),
 .UNSPECIFIED. ) ;
#1026 = B_SPLINE_CURVE_WITH_KNOTS ( 'NONE', 3,
 ( #6744, #3958, #2717, #1593 ),
 .UNSPECIFIED., .F., .F.,
 ( 4, 4 ),
 ( 0.000000000000000000, 1.000000000000000000 ),
 .UNSPECIFIED. ) ;
#1027 = CARTESIAN_POINT ( 'NONE',  ( 17.79267347262679522, -39.86682724249966014, 3.626282107859409187 ) ) ;
#1028 = DIRECTION ( 'NONE',  ( 0.2223157560262043198, -0.6712493609847984821, 0.7071067811865453523 ) ) ;
#1029 = DIRECTION ( 'NONE',  ( -0.9999836672264332815, 0.005715354789859956701, 0.000000000000000000 ) ) ;
#1030 = CARTESIAN_POINT ( 'NONE',  ( 4.128395891713080523, -66.51223636356003510, -1.999098658498605019 ) ) ;
#1031 = EDGE_CURVE ( 'NONE', #2186, #1044, #5088, .T. ) ;
#1032 = DIRECTION ( 'NONE',  ( -3.391455187862681927E-16, -1.191495097990696953E-15, 1.000000000000000000 ) ) ;
#1033 = VERTEX_POINT ( 'NONE', #36 ) ;
#1034 = CARTESIAN_POINT ( 'NONE',  ( -12.11759654540111875, 13.15705282150456945, 1.301042606982605321E-14 ) ) ;
#1035 = CARTESIAN_POINT ( 'NONE',  ( -4.410792138572509735, -62.95272468751611683, 0.08690264739508006542 ) ) ;
#1036 = CARTESIAN_POINT ( 'NONE',  ( -35.54168210215661361, 14.82156649444488394, -1.500000000001999956 ) ) ;
#1037 = DIRECTION ( 'NONE',  ( -0.2023178344681514362, 0.9793199139485103677, 9.781476007338052840E-16 ) ) ;
#1038 = CARTESIAN_POINT ( 'NONE',  ( -4.317466541193835106, -57.77653723152862142, 0.4415034884863752729 ) ) ;
#1039 = CARTESIAN_POINT ( 'NONE',  ( 12.15447797363371052, 11.01039466689934798, -3.299999999999988720 ) ) ;
#1040 = EDGE_CURVE ( 'NONE', #6066, #5379, #3381, .T. ) ;
#1041 = CARTESIAN_POINT ( 'NONE',  ( -0.4891006619385195320, -66.67017596358577691, -1.083201131225852265 ) ) ;
#1042 = ORIENTED_EDGE ( 'NONE', *, *, #5917, .T. ) ;
#1043 = EDGE_CURVE ( 'NONE', #1750, #4040, #3536, .T. ) ;
#1044 = VERTEX_POINT ( 'NONE', #4646 ) ;
#1045 = EDGE_LOOP ( 'NONE', ( #4028, #1415, #2287, #784, #2380, #4918 ) ) ;
#1046 = EDGE_LOOP ( 'NONE', ( #6190, #5981, #4892, #6244 ) ) ;
#1047 = DIRECTION ( 'NONE',  ( 0.9999836672264333925, -0.005715354789844381486, 0.000000000000000000 ) ) ;
#1048 = ORIENTED_EDGE ( 'NONE', *, *, #3659, .F. ) ;
#1049 = DIRECTION ( 'NONE',  ( -1.602374898470634869E-16, 1.442524254523139935E-17, 1.000000000000000000 ) ) ;
#1050 = DIRECTION ( 'NONE',  ( 0.9999836672264335036, -0.005715354789845041548, 0.000000000000000000 ) ) ;
#1051 = CARTESIAN_POINT ( 'NONE',  ( -5.957512881900739465, -64.40555820178136059, 2.727170671215090270 ) ) ;
#1052 = ORIENTED_EDGE ( 'NONE', *, *, #2646, .F. ) ;
#1053 = EDGE_CURVE ( 'NONE', #507, #3368, #677, .T. ) ;
#1054 = ORIENTED_EDGE ( 'NONE', *, *, #3325, .F. ) ;
#1055 = DIRECTION ( 'NONE',  ( -3.391455187862681927E-16, -1.191495097990696953E-15, 1.000000000000000000 ) ) ;
#1056 = FACE_OUTER_BOUND ( 'NONE', #2951, .T. ) ;
#1057 = CARTESIAN_POINT ( 'NONE',  ( -6.308476396955129850, -59.14191327212131455, -0.5142043607924547954 ) ) ;
#1058 = LINE ( 'NONE', #6298, #1020 ) ;
#1059 = CARTESIAN_POINT ( 'NONE',  ( 27.81639631407590585, -34.74023945865230445, 3.614623298852130517 ) ) ;
#1060 = DIRECTION ( 'NONE',  ( 0.9999836672264331705, -0.005715354789860001804, 0.000000000000000000 ) ) ;
#1061 = ORIENTED_EDGE ( 'NONE', *, *, #2233, .T. ) ;
#1062 = ORIENTED_EDGE ( 'NONE', *, *, #621, .F. ) ;
#1063 = CARTESIAN_POINT ( 'NONE',  ( 18.31450325791856315, -40.15738803827605352, 3.873838653338203208 ) ) ;
#1064 = CARTESIAN_POINT ( 'NONE',  ( 43.95483829995806957, -94.87490738911687060, 2.999999999999905409 ) ) ;
#1065 = CYLINDRICAL_SURFACE ( 'NONE', #6259, 17.99999999999999645 ) ;
#1066 = CARTESIAN_POINT ( 'NONE',  ( 7.124841322228030904, -62.19900605811294980, -0.1440571144897197509 ) ) ;
#1067 = DIRECTION ( 'NONE',  ( -5.715354789860003484E-18, -9.999836672264337477E-16, 1.000000000000000000 ) ) ;
#1068 = ORIENTED_EDGE ( 'NONE', *, *, #5637, .T. ) ;
#1069 = DIRECTION ( 'NONE',  ( -5.715354789845005112E-18, -9.999836672264339449E-16, 1.000000000000000000 ) ) ;
#1070 = CARTESIAN_POINT ( 'NONE',  ( 4.447965418036755381, -62.61493371638615457, -2.739923498411994451 ) ) ;
#1071 = EDGE_CURVE ( 'NONE', #3368, #3946, #5330, .T. ) ;
#1072 = CARTESIAN_POINT ( 'NONE',  ( 27.68174825049008803, -37.24611774345110859, 2.999999999999962697 ) ) ;
#1073 = PLANE ( 'NONE',  #1248 ) ;
#1074 = TOROIDAL_SURFACE ( 'NONE', #2746, 140.0000000000000000, 1.000000000000000000 ) ;
#1075 = CARTESIAN_POINT ( 'NONE',  ( -9.358272925367041140, -51.27205205187813419, 2.526284428608170263 ) ) ;
#1076 = CARTESIAN_POINT ( 'NONE',  ( -5.318175601589866908, -63.71090186687732171, -0.7685412544916830901 ) ) ;
#1077 = CARTESIAN_POINT ( 'NONE',  ( -6.338727533122220592, -59.01378846946391832, -2.577673957235475211 ) ) ;
#1078 = ORIENTED_EDGE ( 'NONE', *, *, #3929, .T. ) ;
#1079 = VERTEX_POINT ( 'NONE', #6501 ) ;
#1080 = ORIENTED_EDGE ( 'NONE', *, *, #1641, .T. ) ;
#1081 = AXIS2_PLACEMENT_3D ( 'NONE', #1259, #3654, #5970 ) ;
#1082 = ADVANCED_FACE ( 'NONE', ( #4781 ), #5572, .F. ) ;
#1083 = ADVANCED_FACE ( 'NONE', ( #1873 ), #5881, .T. ) ;
#1084 = DIRECTION ( 'NONE',  ( 0.3866393274467394559, -0.9222310071080526139, -9.200061635857666883E-16 ) ) ;
#1085 = FACE_OUTER_BOUND ( 'NONE', #5107, .T. ) ;
#1086 = PLANE ( 'NONE',  #50 ) ;
#1087 = DIRECTION ( 'NONE',  ( 5.715354789845005112E-18, 9.999836672264339449E-16, -1.000000000000000000 ) ) ;
#1088 = CARTESIAN_POINT ( 'NONE',  ( -3.941959611298590183, -54.25574829393653431, -0.9393447306324897994 ) ) ;
#1089 = VERTEX_POINT ( 'NONE', #737 ) ;
#1090 = AXIS2_PLACEMENT_3D ( 'NONE', #4036, #2774, #6774 ) ;
#1091 = CYLINDRICAL_SURFACE ( 'NONE', #6752, 0.9999999999999988898 ) ;
#1092 = FACE_OUTER_BOUND ( 'NONE', #2421, .T. ) ;
#1093 = EDGE_CURVE ( 'NONE', #184, #3517, #4210, .T. ) ;
#1094 = DIRECTION ( 'NONE',  ( 5.715354789845005112E-18, 9.999836672264339449E-16, -1.000000000000000000 ) ) ;
#1095 = AXIS2_PLACEMENT_3D ( 'NONE', #499, #2173, #4448 ) ;
#1096 = CARTESIAN_POINT ( 'NONE',  ( -34.88460058024264043, 16.28046363954882736, -1.493845543551999944 ) ) ;
#1097 = CARTESIAN_POINT ( 'NONE',  ( -108.8601514936008385, -112.6033348200152773, 3.499999999999886757 ) ) ;
#1098 = DIRECTION ( 'NONE',  ( -5.715354789845005112E-18, -9.999836672264339449E-16, 1.000000000000000000 ) ) ;
#1099 = ORIENTED_EDGE ( 'NONE', *, *, #1810, .F. ) ;
#1100 = CIRCLE ( 'NONE', #3980, 0.9999999999999986677 ) ;
#1101 = ORIENTED_EDGE ( 'NONE', *, *, #3974, .T. ) ;
#1102 = DIRECTION ( 'NONE',  ( 0.9999836672264332815, -0.005715354789845002517, 0.000000000000000000 ) ) ;
#1103 = CARTESIAN_POINT ( 'NONE',  ( -32.59768532061886503, 15.27050393970963782, -2.243845543551999722 ) ) ;
#1104 = CARTESIAN_POINT ( 'NONE',  ( -15.08175531864075047, -33.26559167236155190, -4.352666404962730162 ) ) ;
#1105 = CARTESIAN_POINT ( 'NONE',  ( -6.238287558858839787, -63.42668406018486849, 1.752565146537014895 ) ) ;
#1106 = CARTESIAN_POINT ( 'NONE',  ( 3.875821393968650330, 20.14928133654075282, 2.038300084272748336E-14 ) ) ;
#1107 = ORIENTED_EDGE ( 'NONE', *, *, #4795, .F. ) ;
#1108 = CARTESIAN_POINT ( 'NONE',  ( -9.311346830843410416, -51.41373841511900622, 1.033728595105000148 ) ) ;
#1109 = CARTESIAN_POINT ( 'NONE',  ( -4.317466541193835106, -57.77653723152862142, 0.4415034884863752729 ) ) ;
#1110 = CARTESIAN_POINT ( 'NONE',  ( -15.00216760413269945, 6.625337177075933504, 3.000000000000006661 ) ) ;
#1111 = APPLICATION_CONTEXT ( 'automotive_design' ) ;
#1112 = DIRECTION ( 'NONE',  ( 0.9147661038495522590, -0.4039838799357101107, 0.000000000000000000 ) ) ;
#1113 = CARTESIAN_POINT ( 'NONE',  ( -1.005393588828258133, -65.41824993351924888, -2.298700180912566449 ) ) ;
#1114 = VECTOR ( 'NONE', #7078, 1000.000000000000114 ) ;
#1115 = DIRECTION ( 'NONE',  ( -0.7411265327553938631, -0.6713653717953943501, -6.570922257487907035E-16 ) ) ;
#1116 = CARTESIAN_POINT ( 'NONE',  ( -6.227481695512121718, -59.47789623974718864, -0.5324849168858507564 ) ) ;
#1117 = ORIENTED_EDGE ( 'NONE', *, *, #1901, .T. ) ;
#1118 = EDGE_CURVE ( 'NONE', #3179, #4706, #4817, .T. ) ;
#1119 = ORIENTED_EDGE ( 'NONE', *, *, #1682, .F. ) ;
#1120 = ORIENTED_EDGE ( 'NONE', *, *, #2536, .F. ) ;
#1121 = AXIS2_PLACEMENT_3D ( 'NONE', #4097, #6930, #7411 ) ;
#1122 = DIRECTION ( 'NONE',  ( 0.9999836672264331705, -0.005715354789862803382, 0.000000000000000000 ) ) ;
#1123 = AXIS2_PLACEMENT_3D ( 'NONE', #4973, #5514, #2057 ) ;
#1124 = VERTEX_POINT ( 'NONE', #1348 ) ;
#1125 = DIRECTION ( 'NONE',  ( 5.715354789845005112E-18, 9.999836672264339449E-16, -1.000000000000000000 ) ) ;
#1126 = CARTESIAN_POINT ( 'NONE',  ( 1.172374092613760022, -4.860610968486169803, -3.500000000000000000 ) ) ;
#1127 = CARTESIAN_POINT ( 'NONE',  ( -8.362056880804429326, -51.09933645781752887, 2.533728595105000370 ) ) ;
#1128 = CARTESIAN_POINT ( 'NONE',  ( -4.101849953070630050, -66.53066707031882743, 2.593177719986650143 ) ) ;
#1129 = AXIS2_PLACEMENT_3D ( 'NONE', #5439, #273, #3766 ) ;
#1130 = CIRCLE ( 'NONE', #3756, 0.5000000000000066613 ) ;
#1131 = EDGE_LOOP ( 'NONE', ( #4538, #294, #3018, #5684 ) ) ;
#1132 = EDGE_CURVE ( 'NONE', #489, #4174, #1353, .T. ) ;
#1133 = ORIENTED_EDGE ( 'NONE', *, *, #6582, .T. ) ;
#1134 = CIRCLE ( 'NONE', #2685, 0.7499999999999893419 ) ;
#1135 = DIRECTION ( 'NONE',  ( -0.1937640608316276714, 0.9810481582114290999, 9.799247046208297627E-16 ) ) ;
#1136 = DIRECTION ( 'NONE',  ( -0.9147661038495505936, 0.4039838799357137744, 3.987490689252539707E-16 ) ) ;
#1137 = VECTOR ( 'NONE', #4984, 999.9999999999998863 ) ;
#1138 = CARTESIAN_POINT ( 'NONE',  ( 14.19688052452437255, 19.82243459985110334, -2.993845543551514776 ) ) ;
#1139 = DIRECTION ( 'NONE',  ( -0.4039838799357192700, -0.9147661038495482622, -8.673617379884158732E-16 ) ) ;
#1140 = VECTOR ( 'NONE', #4420, 1000.000000000000000 ) ;
#1141 = CARTESIAN_POINT ( 'NONE',  ( -20.16480223318149356, 14.61937842657788345, -2.993845543551524990 ) ) ;
#1142 = LINE ( 'NONE', #2372, #5672 ) ;
#1143 = VERTEX_POINT ( 'NONE', #186 ) ;
#1144 = EDGE_CURVE ( 'NONE', #909, #3946, #702, .T. ) ;
#1145 = EDGE_CURVE ( 'NONE', #5783, #2991, #872, .T. ) ;
#1146 = ORIENTED_EDGE ( 'NONE', *, *, #3847, .F. ) ;
#1147 = CIRCLE ( 'NONE', #5355, 0.7500000000000000000 ) ;
#1148 = CARTESIAN_POINT ( 'NONE',  ( -7.672523287152989369, -8.566351989504941145, 2.999999999999991562 ) ) ;
#1149 = PLANE ( 'NONE',  #3041 ) ;
#1150 = CARTESIAN_POINT ( 'NONE',  ( 26.82878048574519525, 24.30342645899339971, 2.428612866367529932E-14 ) ) ;
#1151 = CARTESIAN_POINT ( 'NONE',  ( -1.432436674628349893, -67.38906872584260555, -2.752582849501530760 ) ) ;
#1152 = CARTESIAN_POINT ( 'NONE',  ( -12.36403222600316276, 10.92614786255227166, -2.999999999999990230 ) ) ;
#1153 = EDGE_CURVE ( 'NONE', #7182, #878, #2435, .T. ) ;
#1154 = ORIENTED_EDGE ( 'NONE', *, *, #5518, .F. ) ;
#1155 = CARTESIAN_POINT ( 'NONE',  ( 31.14423615379030608, -4.720863734206126594, -4.336808689942017736E-15 ) ) ;
#1156 = DIRECTION ( 'NONE',  ( -0.8039121061460990925, 0.3550279469270785637, -0.4771587602596087385 ) ) ;
#1157 = CARTESIAN_POINT ( 'NONE',  ( -24.22739558392570203, 5.420192826457481239, 3.306154456448477497 ) ) ;
#1158 = CARTESIAN_POINT ( 'NONE',  ( 2.753836159791509974, -65.67748394244114252, 3.050484385245309849 ) ) ;
#1159 = DIRECTION ( 'NONE',  ( -2.925622616928933849E-16, -1.164954066665946421E-15, 1.000000000000000000 ) ) ;
#1160 = CARTESIAN_POINT ( 'NONE',  ( -4.053309352542619592, -65.19933310964161421, -0.8734501311131982471 ) ) ;
#1161 = ORIENTED_EDGE ( 'NONE', *, *, #4113, .T. ) ;
#1162 = EDGE_LOOP ( 'NONE', ( #4430, #5001, #2658, #3993 ) ) ;
#1163 = EDGE_LOOP ( 'NONE', ( #5384, #1864 ) ) ;
#1164 = SHAPE_DEFINITION_REPRESENTATION ( #1991, #3150 ) ;
#1165 = DIRECTION ( 'NONE',  ( 0.7411265327553913096, 0.6713653717953970146, 6.200790563844063010E-16 ) ) ;
#1166 = CYLINDRICAL_SURFACE ( 'NONE', #527, 0.5000000000000004441 ) ;
#1167 = CARTESIAN_POINT ( 'NONE',  ( -1.985532163257450078, -53.63691243282757881, -1.870211432998861945 ) ) ;
#1168 = CARTESIAN_POINT ( 'NONE',  ( 27.55792021817859805, -34.88417811465595264, -0.8737629652053834350 ) ) ;
#1169 = CARTESIAN_POINT ( 'NONE',  ( 5.271413390890690387, -61.79997272665566044, -1.279516964844005900 ) ) ;
#1170 = VERTEX_POINT ( 'NONE', #4747 ) ;
#1171 = ORIENTED_EDGE ( 'NONE', *, *, #1304, .F. ) ;
#1172 = FILL_AREA_STYLE_COLOUR ( '', #4123 ) ;
#1173 = FACE_OUTER_BOUND ( 'NONE', #4086, .T. ) ;
#1174 = ADVANCED_FACE ( 'NONE', ( #2548 ), #6577, .T. ) ;
#1175 = DIRECTION ( 'NONE',  ( 0.9147661038495520369, -0.4039838799357104437, -3.987490689252506674E-16 ) ) ;
#1176 = DIRECTION ( 'NONE',  ( -0.3213584079436493934, 0.3547505615521249767, -0.8779981849197497912 ) ) ;
#1177 = CARTESIAN_POINT ( 'NONE',  ( -105.7473861751082040, -118.0666774205683822, 3.999999999999881428 ) ) ;
#1178 = CARTESIAN_POINT ( 'NONE',  ( 10.30762257547189975, -51.58645851951763461, -2.495037190209991707 ) ) ;
#1179 = EDGE_LOOP ( 'NONE', ( #1416, #4551, #7282, #4937 ) ) ;
#1180 = EDGE_CURVE ( 'NONE', #1972, #123, #157, .T. ) ;
#1181 = CARTESIAN_POINT ( 'NONE',  ( 18.44231076305980466, -39.49669331989797172, 3.499999956044343552 ) ) ;
#1182 = EDGE_CURVE ( 'NONE', #6822, #2064, #5580, .T. ) ;
#1183 = LINE ( 'NONE', #7383, #760 ) ;
#1184 = CARTESIAN_POINT ( 'NONE',  ( -5.205673437485017097, -63.09603712129732855, 1.507649522180431800 ) ) ;
#1185 = CARTESIAN_POINT ( 'NONE',  ( 5.396949887678069935, -64.06165292293543700, 0.6913201402231599069 ) ) ;
#1186 = CYLINDRICAL_SURFACE ( 'NONE', #3650, 0.7500000000000000000 ) ;
#1187 = EDGE_LOOP ( 'NONE', ( #5457, #3397, #3061, #6621, #1235 ) ) ;
#1188 = CARTESIAN_POINT ( 'NONE',  ( -5.011296251047005157, -62.10358530323204462, 3.211213581958491492 ) ) ;
#1189 = DIRECTION ( 'NONE',  ( -0.9879743132267160277, -0.1546180985661085583, 0.000000000000000000 ) ) ;
#1190 = DIRECTION ( 'NONE',  ( -0.1248576012279878633, 0.9921746718272910215, 1.096417580487672448E-15 ) ) ;
#1191 = ADVANCED_FACE ( 'NONE', ( #5992 ), #142, .F. ) ;
#1192 = DIRECTION ( 'NONE',  ( -0.3963837160139272453, -0.9180849359830441925, -9.203354146796070219E-16 ) ) ;
#1193 = CARTESIAN_POINT ( 'NONE',  ( -5.689067437457130616, -61.48253059702771850, 3.675478928603590489 ) ) ;
#1194 = DIRECTION ( 'NONE',  ( -0.2467992669038191478, 0.02032136184815930280, 0.9688535307818069153 ) ) ;
#1195 = DIRECTION ( 'NONE',  ( 0.2223157560262044585, -0.6712493609847989262, 0.7071067811865449082 ) ) ;
#1196 = EDGE_LOOP ( 'NONE', ( #6566, #5335, #307, #6567 ) ) ;
#1197 = ORIENTED_EDGE ( 'NONE', *, *, #7043, .T. ) ;
#1198 = VERTEX_POINT ( 'NONE', #6993 ) ;
#1199 = CARTESIAN_POINT ( 'NONE',  ( 13.19545720709724890, -35.82600185752891520, 2.999999999999964473 ) ) ;
#1200 = EDGE_CURVE ( 'NONE', #5032, #2317, #7140, .T. ) ;
#1201 = DIRECTION ( 'NONE',  ( 0.7411265327553913096, 0.6713653717953970146, 6.200790563844063010E-16 ) ) ;
#1202 = CARTESIAN_POINT ( 'NONE',  ( -2.104778383727555102, -66.59261038346899397, 1.133408834283370137 ) ) ;
#1203 = FACE_OUTER_BOUND ( 'NONE', #5268, .T. ) ;
#1204 = CARTESIAN_POINT ( 'NONE',  ( 2.734303695691099989, -65.14978033110251943, -1.014598242344157963 ) ) ;
#1205 = B_SPLINE_CURVE_WITH_KNOTS ( 'NONE', 3,
 ( #5469, #3072, #7099, #5994, #5388, #2513, #4820, #4251, #4524, #1684 ),
 .UNSPECIFIED., .F., .F.,
 ( 4, 2, 2, 2, 4 ),
 ( 0.000000000000000000, 0.2500000000000002776, 0.5000000000000002220, 0.7500000000000001110, 1.000000000000000000 ),
 .UNSPECIFIED. ) ;
#1206 = ORIENTED_EDGE ( 'NONE', *, *, #104, .F. ) ;
#1207 = AXIS2_PLACEMENT_3D ( 'NONE', #974, #6622, #5516 ) ;
#1208 = CARTESIAN_POINT ( 'NONE',  ( 14.38237858429363492, 13.02858623836822005, 2.236547809770392359 ) ) ;
#1209 = CARTESIAN_POINT ( 'NONE',  ( 19.86817077757012484, -41.71399671145084653, -4.163336342344337027E-14 ) ) ;
#1210 = CARTESIAN_POINT ( 'NONE',  ( -7.741417275248890562, 12.33509147838778475, 3.000000000000011990 ) ) ;
#1211 = VECTOR ( 'NONE', #5626, 1000.000000000000114 ) ;
#1212 = DIRECTION ( 'NONE',  ( -0.9147661038495487063, 0.4039838799357181043, 3.987490689252446030E-16 ) ) ;
#1213 = CARTESIAN_POINT ( 'NONE',  ( 3.403992074353090036, -54.97443010399496899, 2.224669212202579960 ) ) ;
#1214 = ORIENTED_EDGE ( 'NONE', *, *, #2963, .F. ) ;
#1215 = ORIENTED_EDGE ( 'NONE', *, *, #111, .T. ) ;
#1216 = ADVANCED_FACE ( 'NONE', ( #1976 ), #1836, .F. ) ;
#1217 = VECTOR ( 'NONE', #4153, 1000.000000000000114 ) ;
#1218 = CARTESIAN_POINT ( 'NONE',  ( -28.32684271132278298, 12.56450996214383409, -1.493845543551522104 ) ) ;
#1219 = CARTESIAN_POINT ( 'NONE',  ( 15.49911764349215026, -35.75048010860329839, 0.4975185951050001831 ) ) ;
#1220 = CARTESIAN_POINT ( 'NONE',  ( 4.719984496330532409, -63.87667799492090381, 0.8260579302787993683 ) ) ;
#1221 = CIRCLE ( 'NONE', #5427, 1.000000000000001110 ) ;
#1222 = DIRECTION ( 'NONE',  ( 0.1628827478269146978, -0.7884342920379695530, 0.5931615105508275532 ) ) ;
#1223 = EDGE_LOOP ( 'NONE', ( #5305, #6325, #1457, #3436 ) ) ;
#1224 = ADVANCED_FACE ( 'NONE', ( #4142 ), #6440, .T. ) ;
#1225 = CARTESIAN_POINT ( 'NONE',  ( -5.078718092191791378, -62.12561931644285806, 3.276649263749329855 ) ) ;
#1226 = PRODUCT_DEFINITION ( 'UNKNOWN', '', #1481, #4879 ) ;
#1227 = CARTESIAN_POINT ( 'NONE',  ( -10.30756287540601868, -51.58645400917961865, 2.526284428608170263 ) ) ;
#1228 = CARTESIAN_POINT ( 'NONE',  ( -1.799724466760814989, -66.07795133246216324, 3.315732812615050484 ) ) ;
#1229 = CARTESIAN_POINT ( 'NONE',  ( -6.308476396955129850, -59.14191327212131455, -0.5142043607924547954 ) ) ;
#1230 = DIRECTION ( 'NONE',  ( -0.1628827478269146978, 0.7884342920379695530, -0.5931615105508275532 ) ) ;
#1231 = VERTEX_POINT ( 'NONE', #2096 ) ;
#1232 = CIRCLE ( 'NONE', #976, 1.100000000000000755 ) ;
#1233 = EDGE_LOOP ( 'NONE', ( #3225, #3020, #728, #6540 ) ) ;
#1234 = ADVANCED_FACE ( 'NONE', ( #3745 ), #5983, .T. ) ;
#1235 = ORIENTED_EDGE ( 'NONE', *, *, #2956, .F. ) ;
#1236 = VERTEX_POINT ( 'NONE', #2622 ) ;
#1237 = DIRECTION ( 'NONE',  ( 1.046706025223848628E-16, -1.111638688234981404E-15, 1.000000000000000000 ) ) ;
#1238 = CIRCLE ( 'NONE', #2899, 1.000000000000001776 ) ;
#1239 = AXIS2_PLACEMENT_3D ( 'NONE', #1108, #1751, #5323 ) ;
#1240 = CARTESIAN_POINT ( 'NONE',  ( -3.381846796090564933, -54.21055914560344746, 0.1632119451740500493 ) ) ;
#1241 = DIRECTION ( 'NONE',  ( 0.3144019573014849023, -0.9492899500389727629, 0.000000000000000000 ) ) ;
#1242 = VECTOR ( 'NONE', #2762, 1000.000000000000000 ) ;
#1243 = ORIENTED_EDGE ( 'NONE', *, *, #2823, .F. ) ;
#1244 = CIRCLE ( 'NONE', #391, 0.5000000000000022204 ) ;
#1245 =( GEOMETRIC_REPRESENTATION_CONTEXT ( 3 ) GLOBAL_UNCERTAINTY_ASSIGNED_CONTEXT ( ( #2459 ) ) GLOBAL_UNIT_ASSIGNED_CONTEXT ( ( #1246, #4176, #141 ) ) REPRESENTATION_CONTEXT ( 'NONE', 'WORKASPACE' ) );
#1246 =( LENGTH_UNIT ( ) NAMED_UNIT ( * ) SI_UNIT ( .MILLI., .METRE. ) );
#1247 = DIRECTION ( 'NONE',  ( -5.715354789860003484E-18, -9.999836672264337477E-16, 1.000000000000000000 ) ) ;
#1248 = AXIS2_PLACEMENT_3D ( 'NONE', #5184, #2307, #5150 ) ;
#1249 = CARTESIAN_POINT ( 'NONE',  ( -14.81339646197689852, -34.80111785677370051, -0.4662714048949997969 ) ) ;
#1250 = AXIS2_PLACEMENT_3D ( 'NONE', #254, #2589, #1387 ) ;
#1251 = CARTESIAN_POINT ( 'NONE',  ( 6.643375263299909683, -62.64442119333418901, -2.502572238011808281 ) ) ;
#1252 = FACE_OUTER_BOUND ( 'NONE', #2627, .T. ) ;
#1253 = VECTOR ( 'NONE', #3013, 1000.000000000000000 ) ;
#1254 = CIRCLE ( 'NONE', #6772, 1.000000000000001110 ) ;
#1255 = CARTESIAN_POINT ( 'NONE',  ( 1.080279179814437773, -65.65553934942860792, 2.784998920779040432 ) ) ;
#1256 = CIRCLE ( 'NONE', #2447, 0.7499999999999994449 ) ;
#1257 = CONICAL_SURFACE ( 'NONE', #2569, 0.7499999999999872324, 1.029744258676647872 ) ;
#1258 = DIRECTION ( 'NONE',  ( 2.290931512739800066E-16, 1.403768413105889815E-16, 1.000000000000000000 ) ) ;
#1259 = CARTESIAN_POINT ( 'NONE',  ( -95.86211798318534250, -102.0316339954322018, 2.999999999999897859 ) ) ;
#1260 = EDGE_CURVE ( 'NONE', #327, #6872, #1366, .T. ) ;
#1261 = LINE ( 'NONE', #1150, #3487 ) ;
#1262 = DIRECTION ( 'NONE',  ( 0.000000000000000000, -0.7252565289002705917, -0.6884787340851793447 ) ) ;
#1263 = AXIS2_PLACEMENT_3D ( 'NONE', #2069, #6089, #3989 ) ;
#1264 = APPLICATION_CONTEXT ( 'automotive_design' ) ;
#1265 = ORIENTED_EDGE ( 'NONE', *, *, #6853, .T. ) ;
#1266 = DIRECTION ( 'NONE',  ( 5.715354789845005112E-18, 9.999836672264339449E-16, -1.000000000000000000 ) ) ;
#1267 = CIRCLE ( 'NONE', #2579, 3.750000000000000000 ) ;
#1268 = CARTESIAN_POINT ( 'NONE',  ( 17.99687608643026593, -40.34751144403527690, -0.5039026972369210489 ) ) ;
#1269 = EDGE_CURVE ( 'NONE', #5341, #5266, #1568, .T. ) ;
#1270 = CARTESIAN_POINT ( 'NONE',  ( -2.889418079045375176, -55.97554976774797098, -0.4852521485111498389 ) ) ;
#1271 = CARTESIAN_POINT ( 'NONE',  ( -6.239404450008960268, -62.05055862403510503, 1.429382062327010150 ) ) ;
#1272 = LINE ( 'NONE', #3552, #4709 ) ;
#1273 = VERTEX_POINT ( 'NONE', #7255 ) ;
#1274 = ORIENTED_EDGE ( 'NONE', *, *, #4073, .F. ) ;
#1275 = ORIENTED_EDGE ( 'NONE', *, *, #7010, .F. ) ;
#1276 = ORIENTED_EDGE ( 'NONE', *, *, #3188, .F. ) ;
#1277 = CARTESIAN_POINT ( 'NONE',  ( 18.04796579205319063, 16.34913706177017900, -2.993845543551523214 ) ) ;
#1278 = EDGE_LOOP ( 'NONE', ( #3386, #355, #6802 ) ) ;
#1279 = FACE_OUTER_BOUND ( 'NONE', #7094, .T. ) ;
#1280 = EDGE_CURVE ( 'NONE', #2431, #1079, #3183, .T. ) ;
#1281 = EDGE_CURVE ( 'NONE', #3216, #6745, #5458, .T. ) ;
#1282 = CARTESIAN_POINT ( 'NONE',  ( -6.079305786110669629, -62.05959118544440400, 1.459294228111509995 ) ) ;
#1283 = CARTESIAN_POINT ( 'NONE',  ( 27.30483170388658110, -34.44723004512043474, -3.833102624698575208E-14 ) ) ;
#1284 = ORIENTED_EDGE ( 'NONE', *, *, #1631, .F. ) ;
#1285 = CARTESIAN_POINT ( 'NONE',  ( 14.29543924104632779, -35.83228874779774742, -3.556183125752454544E-14 ) ) ;
#1286 = ADVANCED_FACE ( 'NONE', ( #3299 ), #1611, .F. ) ;
#1287 = FACE_OUTER_BOUND ( 'NONE', #365, .T. ) ;
#1288 = DIRECTION ( 'NONE',  ( -0.8748844214391259255, 0.1369338178966306718, -0.4645711771509057897 ) ) ;
#1289 = CARTESIAN_POINT ( 'NONE',  ( 12.26605808802378661, -5.710507655519335479, -3.000000000000006661 ) ) ;
#1290 = CARTESIAN_POINT ( 'NONE',  ( -4.721082446365287844, -64.53544812894149629, 1.276903664564835283 ) ) ;
#1291 = CARTESIAN_POINT ( 'NONE',  ( -2.437747074861595031, -55.99259917890189797, 0.6173017669495700632 ) ) ;
#1292 = CARTESIAN_POINT ( 'NONE',  ( -4.860610968486169803, -1.172374092613760022, 3.000000000000000000 ) ) ;
#1293 = CARTESIAN_POINT ( 'NONE',  ( 18.04796579205319063, 16.34913706177017900, -2.993845543551572952 ) ) ;
#1294 = CARTESIAN_POINT ( 'NONE',  ( -4.119466531011084065, -64.51282121827222227, -0.6949236412976698141 ) ) ;
#1295 = ORIENTED_EDGE ( 'NONE', *, *, #5654, .T. ) ;
#1296 = CARTESIAN_POINT ( 'NONE',  ( -14.07431766324680034, -37.03265636863024923, 1.026284428608169819 ) ) ;
#1297 = DIRECTION ( 'NONE',  ( -0.4950421911735689018, 0.8688689365825386091, 0.000000000000000000 ) ) ;
#1298 = CARTESIAN_POINT ( 'NONE',  ( 3.069422284440780135, -65.49896014417400636, 0.9299900502622647780 ) ) ;
#1299 = CARTESIAN_POINT ( 'NONE',  ( 5.929218414971320072, -62.35084102844776055, -1.530333388185332932 ) ) ;
#1300 = DIRECTION ( 'NONE',  ( -0.4039838799357108323, -0.9147661038495518149, -9.170600743851223106E-16 ) ) ;
#1301 = ORIENTED_EDGE ( 'NONE', *, *, #4208, .F. ) ;
#1302 = ORIENTED_EDGE ( 'NONE', *, *, #536, .F. ) ;
#1303 = ORIENTED_EDGE ( 'NONE', *, *, #3724, .T. ) ;
#1304 = EDGE_CURVE ( 'NONE', #89, #4550, #2438, .T. ) ;
#1305 = CARTESIAN_POINT ( 'NONE',  ( 0.000000000000000000, 0.000000000000000000, -17.67054229618195293 ) ) ;
#1306 = ORIENTED_EDGE ( 'NONE', *, *, #4864, .T. ) ;
#1307 = DIRECTION ( 'NONE',  ( -5.715354789845005112E-18, -9.999836672264339449E-16, 1.000000000000000000 ) ) ;
#1308 = CARTESIAN_POINT ( 'NONE',  ( 1.600318488538475137, -66.74162401608067796, -1.164216807110747931 ) ) ;
#1309 = DIRECTION ( 'NONE',  ( -0.9999836672264335036, 0.005715354789845041548, 0.000000000000000000 ) ) ;
#1310 = EDGE_LOOP ( 'NONE', ( #6388, #5982, #1827, #6956 ) ) ;
#1311 = ORIENTED_EDGE ( 'NONE', *, *, #111, .F. ) ;
#1312 = ORIENTED_EDGE ( 'NONE', *, *, #7327, .F. ) ;
#1313 = ADVANCED_FACE ( 'NONE', ( #2049 ), #6174, .F. ) ;
#1314 = EDGE_CURVE ( 'NONE', #1124, #1044, #1533, .T. ) ;
#1315 = DIRECTION ( 'NONE',  ( -0.4039838799357163279, -0.9147661038495494834, -8.673617379884193244E-16 ) ) ;
#1316 = DIRECTION ( 'NONE',  ( -0.9879743132267160277, -0.1546180985661085583, -1.602621969470663276E-16 ) ) ;
#1317 = CARTESIAN_POINT ( 'NONE',  ( -10.41850315652351533, -32.21925899276746463, -3.227827820482467005E-14 ) ) ;
#1318 = DIRECTION ( 'NONE',  ( -5.715354789845005112E-18, -9.999836672264339449E-16, 1.000000000000000000 ) ) ;
#1319 = LINE ( 'NONE', #4889, #859 ) ;
#1320 = VECTOR ( 'NONE', #1880, 1000.000000000000000 ) ;
#1321 = ADVANCED_FACE ( 'NONE', ( #5573 ), #6181, .T. ) ;
#1322 = CARTESIAN_POINT ( 'NONE',  ( -1.799724466760814989, -66.07795133246216324, 3.315732812615050484 ) ) ;
#1323 = CARTESIAN_POINT ( 'NONE',  ( -34.88460058024264043, 16.28046363954882736, -1.493845543551999944 ) ) ;
#1324 = LINE ( 'NONE', #652, #1320 ) ;
#1325 = CARTESIAN_POINT ( 'NONE',  ( 5.537683946240698596, -62.28623092199279654, -1.376834937089043809 ) ) ;
#1326 = CARTESIAN_POINT ( 'NONE',  ( 1.211170193666210038, -66.82801115824167937, 0.9562527914032201704 ) ) ;
#1327 = CIRCLE ( 'NONE', #833, 0.9999999999999984457 ) ;
#1328 = ORIENTED_EDGE ( 'NONE', *, *, #7328, .F. ) ;
#1329 = LINE ( 'NONE', #270, #3743 ) ;
#1330 = AXIS2_PLACEMENT_3D ( 'NONE', #2240, #6279, #1230 ) ;
#1331 = DIRECTION ( 'NONE',  ( 0.3144066910790619951, 0.9492883822130741001, 0.000000000000000000 ) ) ;
#1332 = CARTESIAN_POINT ( 'NONE',  ( 18.06432743677800445, -39.71205110999872545, -0.06542542002766411902 ) ) ;
#1333 = CARTESIAN_POINT ( 'NONE',  ( 6.285636693253979779, -59.03245517747429716, 2.489777307435960374 ) ) ;
#1334 = CARTESIAN_POINT ( 'NONE',  ( 4.697834216849050115, -63.19072998194386059, -1.190263883463073880 ) ) ;
#1335 = CARTESIAN_POINT ( 'NONE',  ( -3.156642594714314853, -54.82761582543010093, 1.871643660998590697 ) ) ;
#1336 = DIRECTION ( 'NONE',  ( 0.9999836672264332815, -0.005715354789859876036, 0.000000000000000000 ) ) ;
#1337 = ORIENTED_EDGE ( 'NONE', *, *, #6426, .F. ) ;
#1338 = ORIENTED_EDGE ( 'NONE', *, *, #3346, .F. ) ;
#1339 = VECTOR ( 'NONE', #3728, 1000.000000000000000 ) ;
#1340 = FACE_OUTER_BOUND ( 'NONE', #6786, .T. ) ;
#1341 = CARTESIAN_POINT ( 'NONE',  ( -28.02385480137132845, 13.25058454003066188, -1.493845543551522104 ) ) ;
#1342 = CARTESIAN_POINT ( 'NONE',  ( 1.340549191775572080, -65.71857943717337491, -0.9252791854465649557 ) ) ;
#1343 = EDGE_CURVE ( 'NONE', #7292, #4706, #4493, .T. ) ;
#1344 = ORIENTED_EDGE ( 'NONE', *, *, #6230, .F. ) ;
#1345 = ORIENTED_EDGE ( 'NONE', *, *, #579, .F. ) ;
#1346 = VECTOR ( 'NONE', #6183, 1000.000000000000000 ) ;
#1347 =( NAMED_UNIT ( * ) PLANE_ANGLE_UNIT ( ) SI_UNIT ( $, .RADIAN. ) );
#1348 = CARTESIAN_POINT ( 'NONE',  ( -12.20412794045469518, -35.68083184586667045, -3.000000000000036415 ) ) ;
#1349 = DIRECTION ( 'NONE',  ( 0.9999836672264333925, -0.005715354789860572528, 0.000000000000000000 ) ) ;
#1350 = CARTESIAN_POINT ( 'NONE',  ( 6.285636693253979779, -59.03245517747429716, 2.489777307435960374 ) ) ;
#1351 = EDGE_CURVE ( 'NONE', #106, #6538, #6419, .T. ) ;
#1352 = ORIENTED_EDGE ( 'NONE', *, *, #2823, .T. ) ;
#1353 = CIRCLE ( 'NONE', #7115, 0.4999999999999985567 ) ;
#1354 = VERTEX_POINT ( 'NONE', #2703 ) ;
#1355 = AXIS2_PLACEMENT_3D ( 'NONE', #1984, #816, #5967 ) ;
#1356 = VECTOR ( 'NONE', #671, 1000.000000000000000 ) ;
#1357 = CARTESIAN_POINT ( 'NONE',  ( 1.711268714270854918, -65.48362256684714566, -1.456162841279315945 ) ) ;
#1358 = AXIS2_PLACEMENT_3D ( 'NONE', #3102, #811, #5464 ) ;
#1359 = SURFACE_STYLE_FILL_AREA ( #4219 ) ;
#1360 = CIRCLE ( 'NONE', #865, 1.000000000000000444 ) ;
#1361 = FACE_OUTER_BOUND ( 'NONE', #57, .T. ) ;
#1362 = EDGE_CURVE ( 'NONE', #7266, #815, #6525, .T. ) ;
#1363 = EDGE_CURVE ( 'NONE', #354, #2698, #1130, .T. ) ;
#1364 = CARTESIAN_POINT ( 'NONE',  ( -1.736694270343700275, -54.87097428782529107, -2.111004410316564162 ) ) ;
#1365 = VECTOR ( 'NONE', #582, 1000.000000000000227 ) ;
#1366 = CIRCLE ( 'NONE', #2320, 2.500000000000000444 ) ;
#1367 = ORIENTED_EDGE ( 'NONE', *, *, #1439, .F. ) ;
#1368 = DIRECTION ( 'NONE',  ( -0.3144019573014849023, 0.9492899500389726519, 0.000000000000000000 ) ) ;
#1369 = DIRECTION ( 'NONE',  ( 0.9999836672264332815, -0.005715354789847320975, 0.000000000000000000 ) ) ;
#1370 = DIRECTION ( 'NONE',  ( -0.9999836672264333925, 0.005715354789844984303, 0.000000000000000000 ) ) ;
#1371 = CARTESIAN_POINT ( 'NONE',  ( -6.239404450008960268, -62.05055862403510503, 1.429382062327010150 ) ) ;
#1372 = CIRCLE ( 'NONE', #2337, 0.9999999999999998890 ) ;
#1373 = B_SPLINE_CURVE_WITH_KNOTS ( 'NONE', 3,
 ( #6229, #2296, #3314, #503 ),
 .UNSPECIFIED., .F., .F.,
 ( 4, 4 ),
 ( 0.000000000000000000, 1.000000000000000000 ),
 .UNSPECIFIED. ) ;
#1374 = CIRCLE ( 'NONE', #2338, 0.9999999999999984457 ) ;
#1375 = DIRECTION ( 'NONE',  ( 1.046706025223848628E-16, -1.111638688234981404E-15, 1.000000000000000000 ) ) ;
#1376 = CARTESIAN_POINT ( 'NONE',  ( 26.67188031194815068, 24.16129507000589172, 0.006154456448489217107 ) ) ;
#1377 = VERTEX_POINT ( 'NONE', #5615 ) ;
#1378 = ORIENTED_EDGE ( 'NONE', *, *, #5609, .T. ) ;
#1379 = CIRCLE ( 'NONE', #7379, 1.000000000000001998 ) ;
#1380 = CARTESIAN_POINT ( 'NONE',  ( -28.26642576027046516, -36.90973657692984489, -3.707068639042112348E-14 ) ) ;
#1381 = DIRECTION ( 'NONE',  ( 0.6713653717953966815, -0.7411265327553919757, -7.372773368101216216E-16 ) ) ;
#1382 = CARTESIAN_POINT ( 'NONE',  ( -2.585448123472324777, -55.65377943239024461, 0.04593497335228470535 ) ) ;
#1383 =( BOUNDED_SURFACE ( )  B_SPLINE_SURFACE ( 3, 2, ( 
 ( #4396, #6133, #958 ),
 ( #5566, #401, #2694 ),
 ( #3894, #5069, #5115 ),
 ( #4013, #6208, #6828 ),
 ( #7352, #618, #7395 ),
 ( #6352, #6867, #1713 ),
 ( #3477, #4546, #5152 ),
 ( #1756, #4052, #7313 ),
 ( #6278, #4512, #5676 ),
 ( #3928, #4627, #6318 ) ),
 .UNSPECIFIED., .F., .F., .F. ) 
 B_SPLINE_SURFACE_WITH_KNOTS ( ( 4, 2, 2, 2, 4 ),
 ( 3, 3 ),
 ( -2.981555974335137194E-18, 0.0001952886961233724105, 0.0003905773922467478025, 0.0005858660883701231675, 0.0007811547844934985324 ),
 ( 0.000000000000000000, 1.000000000000000000 ),
 .UNSPECIFIED. ) 
 GEOMETRIC_REPRESENTATION_ITEM ( )  RATIONAL_B_SPLINE_SURFACE ( (
 ( 1.000000000000000000, 0.7001503461741274137, 1.000000000000000000),
 ( 1.000000000000000000, 0.7001491056773789801, 1.000000000000000000),
 ( 1.000000000000000000, 0.7003313827919757095, 1.000000000000000000),
 ( 1.000000000000000000, 0.7010298770397929147, 1.000000000000000000),
 ( 1.000000000000000000, 0.7015467090662059757, 1.000000000000000000),
 ( 1.000000000000000000, 0.7028299121717020981, 1.000000000000000000),
 ( 1.000000000000000000, 0.7036054228162287316, 1.000000000000000000),
 ( 1.000000000000000000, 0.7052774926288423174, 1.000000000000000000),
 ( 1.000000000000000000, 0.7061929979163744653, 1.000000000000000000),
 ( 1.000000000000000000, 0.7071067811865477948, 1.000000000000000000) ) ) 
 REPRESENTATION_ITEM ( '' )  SURFACE ( )  );
#1384 = ORIENTED_EDGE ( 'NONE', *, *, #2180, .T. ) ;
#1385 = ORIENTED_EDGE ( 'NONE', *, *, #4441, .T. ) ;
#1386 =( NAMED_UNIT ( * ) SI_UNIT ( $, .STERADIAN. ) SOLID_ANGLE_UNIT ( ) );
#1387 = DIRECTION ( 'NONE',  ( -0.1950386857152336950, 0.001114733493296387375, 0.9807949166078060443 ) ) ;
#1388 = CARTESIAN_POINT ( 'NONE',  ( -31.91091272472834817, 16.82560631625344172, -2.993845543551523214 ) ) ;
#1389 = CARTESIAN_POINT ( 'NONE',  ( -35.54168210215661361, 14.82156649444488394, -1.500000000001999956 ) ) ;
#1390 = CARTESIAN_POINT ( 'NONE',  ( -5.799935258789999715, -64.30794688765904255, -0.8981536636440297094 ) ) ;
#1391 = ORIENTED_EDGE ( 'NONE', *, *, #1587, .F. ) ;
#1392 = EDGE_CURVE ( 'NONE', #4056, #1930, #444, .T. ) ;
#1393 = CARTESIAN_POINT ( 'NONE',  ( -3.268634523084565036, -65.37612200555487618, 3.404282007464019877 ) ) ;
#1394 = PLANE ( 'NONE',  #3148 ) ;
#1395 = CARTESIAN_POINT ( 'NONE',  ( 10.07902270299396008, 17.77910117033601978, 2.236547809770398132 ) ) ;
#1396 = CARTESIAN_POINT ( 'NONE',  ( -0.3939081796060026619, -54.66775925573097084, -2.032307766995797405 ) ) ;
#1397 = B_SPLINE_SURFACE_WITH_KNOTS ( 'NONE', 1, 3, ( 
 ( #1558, #3846, #1489, #2614 ),
 ( #6603, #7205, #4350, #438 ) ),
 .UNSPECIFIED., .F., .F., .F.,
 ( 2, 2 ),
 ( 4, 4 ),
 ( 0.000000000000000000, 1.000000000000000000 ),
 ( 0.000000000000000000, 1.000000000000000000 ),
 .UNSPECIFIED. ) ;
#1398 = EDGE_LOOP ( 'NONE', ( #6951, #3861 ) ) ;
#1399 = CARTESIAN_POINT ( 'NONE',  ( 14.04314992439729970, -37.12718381969609993, 4.336808689942017736E-16 ) ) ;
#1400 = EDGE_CURVE ( 'NONE', #1506, #4731, #5036, .T. ) ;
#1401 = FACE_OUTER_BOUND ( 'NONE', #771, .T. ) ;
#1402 = CARTESIAN_POINT ( 'NONE',  ( 0.000000000000000000, 0.000000000000000000, -3.000000000000000000 ) ) ;
#1403 = CARTESIAN_POINT ( 'NONE',  ( -5.206993624623629913, -63.95781028998001716, 3.417603084305509853 ) ) ;
#1404 = CARTESIAN_POINT ( 'NONE',  ( -1.735723365167664900, -67.19411771835910940, 0.9573769032209800134 ) ) ;
#1405 = DIRECTION ( 'NONE',  ( 0.9492899500389726519, 0.3144019573014848468, 0.000000000000000000 ) ) ;
#1406 = ORIENTED_EDGE ( 'NONE', *, *, #226, .T. ) ;
#1407 = ORIENTED_EDGE ( 'NONE', *, *, #4065, .F. ) ;
#1408 = ORIENTED_EDGE ( 'NONE', *, *, #7380, .T. ) ;
#1409 = EDGE_CURVE ( 'NONE', #6990, #1914, #3873, .T. ) ;
#1410 = LINE ( 'NONE', #1380, #3507 ) ;
#1411 = CARTESIAN_POINT ( 'NONE',  ( 24.99346688245966419, 26.01411140189437532, -2.993845543551503674 ) ) ;
#1412 = CARTESIAN_POINT ( 'NONE',  ( -1.334494426138621792, -66.80443255658586565, -3.107681693547102775 ) ) ;
#1413 = CARTESIAN_POINT ( 'NONE',  ( -0.5105056437457926588, -54.21698483991842465, -0.08672375508415011702 ) ) ;
#1414 = VERTEX_POINT ( 'NONE', #6324 ) ;
#1415 = ORIENTED_EDGE ( 'NONE', *, *, #4679, .T. ) ;
#1416 = ORIENTED_EDGE ( 'NONE', *, *, #2598, .F. ) ;
#1417 = EDGE_LOOP ( 'NONE', ( #406, #6220, #5612, #7354 ) ) ;
#1418 = CARTESIAN_POINT ( 'NONE',  ( -105.7473861751082040, -118.0666774205683822, 3.999999999999881428 ) ) ;
#1419 = CARTESIAN_POINT ( 'NONE',  ( 0.000000000000000000, 0.000000000000000000, 3.000000000000000000 ) ) ;
#1420 = DIRECTION ( 'NONE',  ( -5.715354789860003484E-18, -9.999836672264337477E-16, 1.000000000000000000 ) ) ;
#1421 = CARTESIAN_POINT ( 'NONE',  ( -3.869447490927095057, -66.24422018797883993, 3.165055290057749993 ) ) ;
#1422 = CARTESIAN_POINT ( 'NONE',  ( 14.97072768011073940, -34.32654753528365177, 2.597518595105000383 ) ) ;
#1423 = CARTESIAN_POINT ( 'NONE',  ( -5.502354252718959948, -62.02724140920135198, 3.641858308670590016 ) ) ;
#1424 = FACE_OUTER_BOUND ( 'NONE', #4705, .T. ) ;
#1425 = DIRECTION ( 'NONE',  ( -5.715354789845005112E-18, -9.999836672264339449E-16, 1.000000000000000000 ) ) ;
#1426 = CARTESIAN_POINT ( 'NONE',  ( -5.784209743144936411, -61.27901533394182110, -2.583004453599333061 ) ) ;
#1427 = EDGE_CURVE ( 'NONE', #1688, #4757, #4669, .T. ) ;
#1428 = ORIENTED_EDGE ( 'NONE', *, *, #6641, .F. ) ;
#1429 = DIRECTION ( 'NONE',  ( 0.3144019573014875113, -0.9492899500389717637, 0.000000000000000000 ) ) ;
#1430 = LINE ( 'NONE', #3720, #3512 ) ;
#1431 = CARTESIAN_POINT ( 'NONE',  ( 14.07443455944474131, -37.03272609524245240, -0.9950371902099899302 ) ) ;
#1432 = DIRECTION ( 'NONE',  ( -0.2467992669038191478, 0.02032136184815930280, 0.9688535307818069153 ) ) ;
#1433 = CARTESIAN_POINT ( 'NONE',  ( 2.986904076224405014, -66.15109244657664078, 2.931604786918900363 ) ) ;
#1434 = FACE_OUTER_BOUND ( 'NONE', #2612, .T. ) ;
#1435 = CIRCLE ( 'NONE', #7326, 1.000000000000001776 ) ;
#1436 = CARTESIAN_POINT ( 'NONE',  ( -7.069128816957480410, -61.66762450778810489, 2.866206824378770168 ) ) ;
#1437 = EDGE_CURVE ( 'NONE', #5266, #4706, #6923, .T. ) ;
#1438 = DIRECTION ( 'NONE',  ( 0.6713653717953944611, -0.7411265327553937521, 8.447904732807262513E-16 ) ) ;
#1439 = EDGE_CURVE ( 'NONE', #1508, #3171, #23, .T. ) ;
#1440 = ORIENTED_EDGE ( 'NONE', *, *, #6555, .T. ) ;
#1441 = VERTEX_POINT ( 'NONE', #6801 ) ;
#1442 = CARTESIAN_POINT ( 'NONE',  ( 24.19069689082242647, 25.28690498020820243, -6.178731080732834613 ) ) ;
#1443 = DIRECTION ( 'NONE',  ( 5.715354789845005112E-18, 9.999836672264339449E-16, -1.000000000000000000 ) ) ;
#1444 = CARTESIAN_POINT ( 'NONE',  ( 5.330483863435800274, -59.34891080545844488, 0.6651839376153853012 ) ) ;
#1445 = CYLINDRICAL_SURFACE ( 'NONE', #2310, 3.750000000000000000 ) ;
#1446 = ADVANCED_FACE ( 'NONE', ( #2279 ), #5096, .T. ) ;
#1447 = CARTESIAN_POINT ( 'NONE',  ( -2.904120812423019782, -54.85523864424144591, 1.880038532258539563 ) ) ;
#1448 = EDGE_CURVE ( 'NONE', #1686, #3666, #1762, .T. ) ;
#1449 = VECTOR ( 'NONE', #7161, 999.9999999999998863 ) ;
#1450 = ORIENTED_EDGE ( 'NONE', *, *, #7191, .F. ) ;
#1451 = ORIENTED_EDGE ( 'NONE', *, *, #6294, .T. ) ;
#1452 = VERTEX_POINT ( 'NONE', #4589 ) ;
#1453 = CARTESIAN_POINT ( 'NONE',  ( -14.97059744062764075, -34.32647288175419931, -2.566271404895000163 ) ) ;
#1454 = CARTESIAN_POINT ( 'NONE',  ( 1.714606436953501688E-17, 2.999951001679301835E-15, 0.000000000000000000 ) ) ;
#1455 = CARTESIAN_POINT ( 'NONE',  ( -9.358272925367041140, -51.27205205187813419, 2.526284428608170263 ) ) ;
#1456 = CARTESIAN_POINT ( 'NONE',  ( 2.080482015124565098, -66.54183146390657555, -1.221303033644861813 ) ) ;
#1457 = ORIENTED_EDGE ( 'NONE', *, *, #1031, .F. ) ;
#1458 = EDGE_CURVE ( 'NONE', #184, #5486, #2499, .T. ) ;
#1459 = ORIENTED_EDGE ( 'NONE', *, *, #6022, .F. ) ;
#1460 = CLOSED_SHELL ( 'NONE', ( #7301, #5880, #2345, #2597, #6498, #6069, #2274, #991, #793, #565, #6071, #6863, #28, #7063, #7051, #902, #68, #6364, #7274, #4952, #6466, #4312, #2583, #1884, #4344, #90, #7432, #4953, #1286, #1224, #6473, #120, #3830, #694, #675, #2964, #6380, #5833, #3888, #1660, #5476, #7096, #4922, #5187, #5314, #7336, #2375, #4215, #4756, #1174, #6875, #893, #1708, #3548, #1313, #5366, #6201, #2864, #2545, #6013, #2757, #1234, #3130, #580, #1996, #6570, #3419, #3564, #5517, #7234, #3002, #6975, #5879, #1216, #4911, #2918, #2493 ) ) ;
#1461 = DIRECTION ( 'NONE',  ( 1.850371707708594760E-14, 4.625929269271487058E-14, -1.000000000000000000 ) ) ;
#1462 = CARTESIAN_POINT ( 'NONE',  ( -1.556563313654149905, -55.35434594439572464, -0.3959639196582302456 ) ) ;
#1463 = EDGE_LOOP ( 'NONE', ( #6688, #2595 ) ) ;
#1464 = AXIS2_PLACEMENT_3D ( 'NONE', #6985, #4168, #1924 ) ;
#1465 = VECTOR ( 'NONE', #6169, 1000.000000000000000 ) ;
#1466 = CARTESIAN_POINT ( 'NONE',  ( -9.311346830843399758, -51.41373841511900622, 2.533728595105000370 ) ) ;
#1467 = CARTESIAN_POINT ( 'NONE',  ( -6.575672653089386976, -62.62123098032723334, 2.148875912808684951 ) ) ;
#1468 = VERTEX_POINT ( 'NONE', #1795 ) ;
#1469 = AXIS2_PLACEMENT_3D ( 'NONE', #7107, #2561, #5617 ) ;
#1470 = B_SPLINE_CURVE_WITH_KNOTS ( 'NONE', 3,
 ( #2814, #2848, #5693, #1576 ),
 .UNSPECIFIED., .F., .F.,
 ( 4, 4 ),
 ( 0.000000000000000000, 1.000000000000000000 ),
 .UNSPECIFIED. ) ;
#1471 = CIRCLE ( 'NONE', #6892, 3.299999999999999378 ) ;
#1472 = AXIS2_PLACEMENT_3D ( 'NONE', #6296, #638, #3948 ) ;
#1473 = ADVANCED_FACE ( 'NONE', ( #2323 ), #2360, .F. ) ;
#1474 = CARTESIAN_POINT ( 'NONE',  ( -33.94153943842304955, 12.25650441806195801, -2.999999999999988898 ) ) ;
#1475 = VECTOR ( 'NONE', #4637, 1000.000000000000114 ) ;
#1476 = CARTESIAN_POINT ( 'NONE',  ( -3.498019654714389581, -55.03494779767484602, -0.2490962732230048438 ) ) ;
#1477 = CARTESIAN_POINT ( 'NONE',  ( -45.28625779897078729, -94.36209361619114588, -3.000000000000095479 ) ) ;
#1478 = AXIS2_PLACEMENT_3D ( 'NONE', #481, #368, #6653 ) ;
#1479 = CARTESIAN_POINT ( 'NONE',  ( -6.822623972396280934, -59.02239909983155286, -0.6330850349556997880 ) ) ;
#1480 = CARTESIAN_POINT ( 'NONE',  ( 14.02750760687355935, -37.17441268192290238, 0.4975185951050001831 ) ) ;
#1481 = PRODUCT_DEFINITION_FORMATION_WITH_SPECIFIED_SOURCE ( 'ANY', '', #846, .NOT_KNOWN. ) ;
#1482 = AXIS2_PLACEMENT_3D ( 'NONE', #4523, #5618, #6724 ) ;
#1483 = ORIENTED_EDGE ( 'NONE', *, *, #1862, .F. ) ;
#1484 = ORIENTED_EDGE ( 'NONE', *, *, #1118, .F. ) ;
#1485 = VECTOR ( 'NONE', #4544, 1000.000000000000000 ) ;
#1486 = DIRECTION ( 'NONE',  ( -0.9999836672264333925, 0.005715354789860572528, 0.000000000000000000 ) ) ;
#1487 = CIRCLE ( 'NONE', #416, 5.000000000000000000 ) ;
#1488 = AXIS2_PLACEMENT_3D ( 'NONE', #3820, #1087, #370 ) ;
#1489 = CARTESIAN_POINT ( 'NONE',  ( 9.290270525626649345, 17.28063226168697497, 2.735643510310428628 ) ) ;
#1490 = CARTESIAN_POINT ( 'NONE',  ( -5.091256589979570535, -61.80182140578926919, 1.697438579844070761 ) ) ;
#1491 = DIRECTION ( 'NONE',  ( -5.715354789860003484E-18, -9.999836672264337477E-16, 1.000000000000000000 ) ) ;
#1492 = CARTESIAN_POINT ( 'NONE',  ( 4.471690325102795072, -64.80734643215984647, 2.824010636486237846 ) ) ;
#1493 = VERTEX_POINT ( 'NONE', #558 ) ;
#1494 = ORIENTED_EDGE ( 'NONE', *, *, #6459, .T. ) ;
#1495 = VECTOR ( 'NONE', #5438, 1000.000000000000227 ) ;
#1496 = ORIENTED_EDGE ( 'NONE', *, *, #7023, .T. ) ;
#1497 = ORIENTED_EDGE ( 'NONE', *, *, #3734, .T. ) ;
#1498 =( REPRESENTATION_RELATIONSHIP ('NONE','NONE', #3195, #5284 ) REPRESENTATION_RELATIONSHIP_WITH_TRANSFORMATION ( #2206 )SHAPE_REPRESENTATION_RELATIONSHIP( ) );
#1499 = EDGE_CURVE ( 'NONE', #2710, #3657, #4057, .T. ) ;
#1500 = CARTESIAN_POINT ( 'NONE',  ( 0.000000000000000000, 0.000000000000000000, 0.000000000000000000 ) ) ;
#1501 = EDGE_CURVE ( 'NONE', #6491, #1414, #1839, .T. ) ;
#1502 = DIRECTION ( 'NONE',  ( 5.715354789845005112E-18, 9.999836672264339449E-16, -1.000000000000000000 ) ) ;
#1503 = CARTESIAN_POINT ( 'NONE',  ( 0.000000000000000000, 0.000000000000000000, -3.000000000000000000 ) ) ;
#1504 = DIRECTION ( 'NONE',  ( -0.005585937530842041351, -0.9773402531220075629, 0.2116006307393995811 ) ) ;
#1505 = CARTESIAN_POINT ( 'NONE',  ( 5.929218414971320072, -62.35084102844776055, -1.530333388185332932 ) ) ;
#1506 = VERTEX_POINT ( 'NONE', #5159 ) ;
#1507 = ORIENTED_EDGE ( 'NONE', *, *, #4985, .T. ) ;
#1508 = VERTEX_POINT ( 'NONE', #6358 ) ;
#1509 = CARTESIAN_POINT ( 'NONE',  ( -20.89962323070193406, -41.21687045383659154, -3.001000000000042078 ) ) ;
#1510 = CARTESIAN_POINT ( 'NONE',  ( -4.908132910216119527, -63.74296424117085991, -0.6604057789239049514 ) ) ;
#1511 = CARTESIAN_POINT ( 'NONE',  ( -35.54168210215661361, 14.82156649444488394, -1.500000000001999956 ) ) ;
#1512 = LINE ( 'NONE', #6623, #4455 ) ;
#1513 = ORIENTED_EDGE ( 'NONE', *, *, #6544, .F. ) ;
#1514 = FACE_OUTER_BOUND ( 'NONE', #7021, .T. ) ;
#1515 = CARTESIAN_POINT ( 'NONE',  ( -34.88460058024264043, 16.28046363954882736, -1.493845543551999944 ) ) ;
#1516 = DIRECTION ( 'NONE',  ( 0.9999836672264332815, -0.005715354789845002517, 0.000000000000000000 ) ) ;
#1517 = CARTESIAN_POINT ( 'NONE',  ( 31.14423615379030608, -4.720863734206129259, 2.999999999999995559 ) ) ;
#1518 = CARTESIAN_POINT ( 'NONE',  ( 43.45632180942044442, -94.90042465344848210, -3.001370543551634906 ) ) ;
#1519 = CARTESIAN_POINT ( 'NONE',  ( 7.168555767344659380, -58.87994835687880624, 1.798531003845740051 ) ) ;
#1520 = CYLINDRICAL_SURFACE ( 'NONE', #3731, 6.300000000000000711 ) ;
#1521 = ORIENTED_EDGE ( 'NONE', *, *, #4334, .T. ) ;
#1522 = VERTEX_POINT ( 'NONE', #1199 ) ;
#1523 = CARTESIAN_POINT ( 'NONE',  ( 1.714606436953501688E-17, 2.999951001679301835E-15, 0.000000000000000000 ) ) ;
#1524 = DIRECTION ( 'NONE',  ( -4.026247463476719020E-15, 1.023028141612472829E-15, -1.000000000000000000 ) ) ;
#1525 = CARTESIAN_POINT ( 'NONE',  ( 2.576047814891095022, -64.81584722952422339, -0.4432308004904150223 ) ) ;
#1526 = LINE ( 'NONE', #7244, #1465 ) ;
#1527 = CARTESIAN_POINT ( 'NONE',  ( 5.863376863421286167, -57.99493907355560651, 0.3327841386862454565 ) ) ;
#1528 = ORIENTED_EDGE ( 'NONE', *, *, #6768, .F. ) ;
#1529 = EDGE_CURVE ( 'NONE', #3340, #1493, #3448, .T. ) ;
#1530 = ORIENTED_EDGE ( 'NONE', *, *, #7183, .T. ) ;
#1531 = ORIENTED_EDGE ( 'NONE', *, *, #3695, .F. ) ;
#1532 = DIRECTION ( 'NONE',  ( 0.000000000000000000, 0.000000000000000000, 1.000000000000000000 ) ) ;
#1533 = LINE ( 'NONE', #4363, #5219 ) ;
#1534 = FACE_OUTER_BOUND ( 'NONE', #5497, .T. ) ;
#1535 = DIRECTION ( 'NONE',  ( 5.715354789845005112E-18, 9.999836672264339449E-16, -1.000000000000000000 ) ) ;
#1536 = CARTESIAN_POINT ( 'NONE',  ( -6.722550792682009835, -58.60332661353002948, 1.487589938850535143 ) ) ;
#1537 = ORIENTED_EDGE ( 'NONE', *, *, #76, .F. ) ;
#1538 = EDGE_LOOP ( 'NONE', ( #6488, #977, #3851, #635, #4519, #6549 ) ) ;
#1539 = EDGE_CURVE ( 'NONE', #6928, #1231, #5117, .T. ) ;
#1540 = EDGE_CURVE ( 'NONE', #6097, #901, #5947, .T. ) ;
#1541 = ORIENTED_EDGE ( 'NONE', *, *, #2264, .F. ) ;
#1542 = PLANE ( 'NONE',  #3149 ) ;
#1543 = CARTESIAN_POINT ( 'NONE',  ( -17.21006346072928750, 13.86884027412869180, -2.230393353321906247 ) ) ;
#1544 = DIRECTION ( 'NONE',  ( 0.2223191033124282123, 0.6712482523644723864, 0.7071067811865472397 ) ) ;
#1545 = CARTESIAN_POINT ( 'NONE',  ( 15.39542127499540136, -35.83857563806657964, 2.999999999999964473 ) ) ;
#1546 = EDGE_CURVE ( 'NONE', #212, #6210, #1678, .T. ) ;
#1547 = VERTEX_POINT ( 'NONE', #7359 ) ;
#1548 = CARTESIAN_POINT ( 'NONE',  ( 15.49911764349215026, -35.75048010860329839, 0.4975185951050001831 ) ) ;
#1549 = DIRECTION ( 'NONE',  ( -5.715354789845005112E-18, -9.999836672264339449E-16, 1.000000000000000000 ) ) ;
#1550 = DIRECTION ( 'NONE',  ( 5.715354789845004342E-18, 9.999836672264337477E-16, -1.000000000000000000 ) ) ;
#1551 = CARTESIAN_POINT ( 'NONE',  ( -6.634274853075190492, -62.58082626503517787, -0.8104611758546799161 ) ) ;
#1552 = CARTESIAN_POINT ( 'NONE',  ( 35.76131148831677109, 4.835142255982176174, -2.999999999999995559 ) ) ;
#1553 = CIRCLE ( 'NONE', #1207, 20.00000000000000711 ) ;
#1554 = ORIENTED_EDGE ( 'NONE', *, *, #6544, .T. ) ;
#1555 = CARTESIAN_POINT ( 'NONE',  ( -14.49899450467539985, -35.75040780681265318, -0.4662714048949997969 ) ) ;
#1556 = DIRECTION ( 'NONE',  ( 0.02358931830619094214, -0.9997217333147505602, -9.995705837626804294E-16 ) ) ;
#1557 = CIRCLE ( 'NONE', #2876, 5.000000000000001776 ) ;
#1558 = CARTESIAN_POINT ( 'NONE',  ( 7.529070345495034289, 16.11642554373085900, 3.000000000000015987 ) ) ;
#1559 = CARTESIAN_POINT ( 'NONE',  ( 5.193956696153660069, -59.28518064773341933, 2.254869812567109832 ) ) ;
#1560 = LINE ( 'NONE', #4925, #4116 ) ;
#1561 = CARTESIAN_POINT ( 'NONE',  ( -1.936202856841531039, -66.43606426736279502, -1.004513860088930732 ) ) ;
#1562 = ORIENTED_EDGE ( 'NONE', *, *, #5909, .T. ) ;
#1563 = CARTESIAN_POINT ( 'NONE',  ( -6.217266535765080704, -62.33106447713396392, -2.754524245347104383 ) ) ;
#1564 = EDGE_LOOP ( 'NONE', ( #7406, #1608, #3074, #586 ) ) ;
#1565 = ORIENTED_EDGE ( 'NONE', *, *, #253, .T. ) ;
#1566 = PRESENTATION_LAYER_ASSIGNMENT (  '', '', ( #1913 ) ) ;
#1567 = CARTESIAN_POINT ( 'NONE',  ( 0.000000000000000000, 0.000000000000000000, 0.000000000000000000 ) ) ;
#1568 = LINE ( 'NONE', #6759, #3154 ) ;
#1569 = EDGE_CURVE ( 'NONE', #3179, #5341, #2207, .T. ) ;
#1570 = FACE_OUTER_BOUND ( 'NONE', #2464, .T. ) ;
#1571 = CARTESIAN_POINT ( 'NONE',  ( -14.63712380658832046, -36.05860345213164919, -4.315410310759999923 ) ) ;
#1572 = CARTESIAN_POINT ( 'NONE',  ( 35.76131148831677109, 4.835142255982176174, -2.999999999999995559 ) ) ;
#1573 = CARTESIAN_POINT ( 'NONE',  ( 4.128395891713080523, -66.51223636356003510, -1.999098658498605019 ) ) ;
#1574 = ORIENTED_EDGE ( 'NONE', *, *, #6150, .T. ) ;
#1575 = ORIENTED_EDGE ( 'NONE', *, *, #6853, .F. ) ;
#1576 = CARTESIAN_POINT ( 'NONE',  ( 9.018117650298766108, 16.81805756487467107, -0.3999035282154979054 ) ) ;
#1577 = CIRCLE ( 'NONE', #4104, 1.100000000000000755 ) ;
#1578 = FACE_OUTER_BOUND ( 'NONE', #5190, .T. ) ;
#1579 = CARTESIAN_POINT ( 'NONE',  ( -5.714251477591489881, -57.46902543231049521, -0.4259505751857597389 ) ) ;
#1580 = CARTESIAN_POINT ( 'NONE',  ( 11.65361085287446663, 10.55667343862480578, 1.040834085586084257E-14 ) ) ;
#1581 = CYLINDRICAL_SURFACE ( 'NONE', #6976, 0.9999999999999984457 ) ;
#1582 = AXIS2_PLACEMENT_3D ( 'NONE', #2900, #6313, #5146 ) ;
#1583 = ORIENTED_EDGE ( 'NONE', *, *, #5545, .F. ) ;
#1584 = ORIENTED_EDGE ( 'NONE', *, *, #4497, .F. ) ;
#1585 = VECTOR ( 'NONE', #4910, 1000.000000000000227 ) ;
#1586 = AXIS2_PLACEMENT_3D ( 'NONE', #6147, #6449, #2490 ) ;
#1587 = EDGE_CURVE ( 'NONE', #6014, #5486, #2985, .T. ) ;
#1588 = CYLINDRICAL_SURFACE ( 'NONE', #5449, 3.750000000000000000 ) ;
#1589 = EDGE_CURVE ( 'NONE', #6736, #2542, #6900, .T. ) ;
#1590 = CARTESIAN_POINT ( 'NONE',  ( 14.63724902514210058, -34.60816281716094522, 2.969700630898919780 ) ) ;
#1591 = DIRECTION ( 'NONE',  ( -0.08966155106958693943, -0.9959722919136836383, 0.000000000000000000 ) ) ;
#1592 = CARTESIAN_POINT ( 'NONE',  ( 6.871427970997950219, -62.19563859352643931, -1.162241389626079702 ) ) ;
#1593 = CARTESIAN_POINT ( 'NONE',  ( 14.63763862841553376, 20.11382921380832656, 0.006154456448485313980 ) ) ;
#1594 = PRESENTATION_LAYER_ASSIGNMENT (  '', '', ( #863 ) ) ;
#1595 = AXIS2_PLACEMENT_3D ( 'NONE', #5939, #63, #4163 ) ;
#1596 = ORIENTED_EDGE ( 'NONE', *, *, #3604, .F. ) ;
#1597 = AXIS2_PLACEMENT_3D ( 'NONE', #3151, #1018, #7330 ) ;
#1598 = CARTESIAN_POINT ( 'NONE',  ( -13.25471347244850051, 13.28966623998220520, -0.1388209971588587888 ) ) ;
#1599 = CARTESIAN_POINT ( 'NONE',  ( -2.332017369136024865, -64.95045318432249815, -2.208845462231724177 ) ) ;
#1600 = DIRECTION ( 'NONE',  ( -5.715354789860003484E-18, -9.999836672264337477E-16, 1.000000000000000000 ) ) ;
#1601 = AXIS2_PLACEMENT_3D ( 'NONE', #5028, #3777, #7311 ) ;
#1602 = EDGE_CURVE ( 'NONE', #4768, #6909, #5340, .T. ) ;
#1603 = VECTOR ( 'NONE', #1165, 1000.000000000000227 ) ;
#1604 = LINE ( 'NONE', #884, #4615 ) ;
#1605 = CARTESIAN_POINT ( 'NONE',  ( -2.332017369136024865, -64.95045318432249815, -2.208845462231724177 ) ) ;
#1606 = DIRECTION ( 'NONE',  ( -5.715354789860003484E-18, -9.999836672264337477E-16, 1.000000000000000000 ) ) ;
#1607 = CARTESIAN_POINT ( 'NONE',  ( 5.091606878585934304, -64.16522473348585720, -1.423946029510006372 ) ) ;
#1608 = ORIENTED_EDGE ( 'NONE', *, *, #6789, .T. ) ;
#1609 = ORIENTED_EDGE ( 'NONE', *, *, #1529, .T. ) ;
#1610 = VECTOR ( 'NONE', #4576, 1000.000000000000114 ) ;
#1611 = CYLINDRICAL_SURFACE ( 'NONE', #2192, 2.999999999999999556 ) ;
#1612 = ORIENTED_EDGE ( 'NONE', *, *, #4124, .T. ) ;
#1613 = CARTESIAN_POINT ( 'NONE',  ( -14.07431766324680034, -37.03265636863024923, 1.026284428608169819 ) ) ;
#1614 = FACE_OUTER_BOUND ( 'NONE', #7315, .T. ) ;
#1615 = CARTESIAN_POINT ( 'NONE',  ( -2.113079283527464991, -53.41662231759018198, -0.8523026345115048974 ) ) ;
#1616 = AXIS2_PLACEMENT_3D ( 'NONE', #4322, #7215, #7098 ) ;
#1617 = CARTESIAN_POINT ( 'NONE',  ( -32.93157973858376408, 14.54341967768581867, -2.999999999999986677 ) ) ;
#1618 = LINE ( 'NONE', #5201, #4369 ) ;
#1619 = CARTESIAN_POINT ( 'NONE',  ( 6.162074140922939591, -62.32076522084695114, 2.666565443060120444 ) ) ;
#1620 = VECTOR ( 'NONE', #3144, 1000.000000000000000 ) ;
#1621 = CARTESIAN_POINT ( 'NONE',  ( -40.82267254781529431, -94.88271315313488685, -9.511447951234663500E-14 ) ) ;
#1622 = DIRECTION ( 'NONE',  ( -5.715354789845005112E-18, -9.999836672264339449E-16, 1.000000000000000000 ) ) ;
#1623 = ORIENTED_EDGE ( 'NONE', *, *, #1963, .F. ) ;
#1624 = ADVANCED_FACE ( 'NONE', ( #5905 ), #6534, .T. ) ;
#1625 = CARTESIAN_POINT ( 'NONE',  ( 18.38544986348231447, -39.52909008669877977, 3.487024505045074996 ) ) ;
#1626 = CARTESIAN_POINT ( 'NONE',  ( 37.86567095459282228, 7.005780695865149177, -1.500000000001998623 ) ) ;
#1627 = FACE_OUTER_BOUND ( 'NONE', #4793, .T. ) ;
#1628 = CARTESIAN_POINT ( 'NONE',  ( 6.939112688521190009, -58.99009576954022549, 0.7806222117286002460 ) ) ;
#1629 = CARTESIAN_POINT ( 'NONE',  ( 18.74668230531428748, -39.89873697698326538, -1.000000000000039968 ) ) ;
#1630 = ORIENTED_EDGE ( 'NONE', *, *, #935, .F. ) ;
#1631 = EDGE_CURVE ( 'NONE', #461, #1922, #3273, .T. ) ;
#1632 = ADVANCED_FACE ( 'NONE', ( #133 ), #2502, .F. ) ;
#1633 = CARTESIAN_POINT ( 'NONE',  ( -15.00216760413269945, 6.625337177075936168, 6.505213034913026604E-15 ) ) ;
#1634 = CARTESIAN_POINT ( 'NONE',  ( -4.302337887170949671, -63.34626699285441020, 3.181678273100430054 ) ) ;
#1635 = CYLINDRICAL_SURFACE ( 'NONE', #5207, 6.299999999999998934 ) ;
#1636 = DIRECTION ( 'NONE',  ( 0.3144019573014853464, -0.9492899500389726519, -7.355227538141627568E-16 ) ) ;
#1637 = CARTESIAN_POINT ( 'NONE',  ( -5.121204309455420045, -61.36711808260334067, 3.320501707867800523 ) ) ;
#1638 = DIRECTION ( 'NONE',  ( 0.2223191033124283789, 0.6712482523644727195, 0.7071067811865466846 ) ) ;
#1639 = CARTESIAN_POINT ( 'NONE',  ( -6.228944513034659458, -61.43090327710801546, -0.6374195285636679031 ) ) ;
#1640 = CARTESIAN_POINT ( 'NONE',  ( 1.014503381694089823, -65.79094358639915185, 1.195300268011630029 ) ) ;
#1641 = EDGE_CURVE ( 'NONE', #2620, #4300, #4234, .T. ) ;
#1642 = ORIENTED_EDGE ( 'NONE', *, *, #4346, .T. ) ;
#1643 = VERTEX_POINT ( 'NONE', #1967 ) ;
#1644 = EDGE_LOOP ( 'NONE', ( #1338, #7251, #6719, #4401, #501 ) ) ;
#1645 = CARTESIAN_POINT ( 'NONE',  ( -14.63712380658832046, -35.33334692323139592, -3.626931576674818025 ) ) ;
#1646 = DIRECTION ( 'NONE',  ( 0.7411265327553895332, 0.6713653717953992350, 6.755902076156661002E-16 ) ) ;
#1647 = DIRECTION ( 'NONE',  ( 0.7411265327553895332, 0.6713653717953992350, 6.755902076156661002E-16 ) ) ;
#1648 = CARTESIAN_POINT ( 'NONE',  ( 3.832282121198885338, -54.47902871778750722, 0.5155147207099053386 ) ) ;
#1649 = ORIENTED_EDGE ( 'NONE', *, *, #837, .F. ) ;
#1650 = EDGE_CURVE ( 'NONE', #7292, #5643, #1410, .T. ) ;
#1651 = CARTESIAN_POINT ( 'NONE',  ( 12.99837876291259064, -32.41640519645540053, -3.252606517456513302E-14 ) ) ;
#1652 = CARTESIAN_POINT ( 'NONE',  ( 27.65482637540493016, -34.83021424519443343, -0.7995430095508657686 ) ) ;
#1653 = CARTESIAN_POINT ( 'NONE',  ( 13.75614703236065672, 19.53106228095526475, -2.928563623636441182 ) ) ;
#1654 = DIRECTION ( 'NONE',  ( 0.6713653717953971256, -0.7411265327553914206, -7.372773368101209313E-16 ) ) ;
#1655 = CARTESIAN_POINT ( 'NONE',  ( 27.57479190627129384, -34.87478370679277617, 3.891341692651370199 ) ) ;
#1656 = PLANE ( 'NONE',  #125 ) ;
#1657 = ORIENTED_EDGE ( 'NONE', *, *, #4539, .T. ) ;
#1658 = CARTESIAN_POINT ( 'NONE',  ( 5.695730293278450596, -62.33055481056936742, -2.502481404895003259 ) ) ;
#1659 = DIRECTION ( 'NONE',  ( -0.5182245224839744369, 0.8552446107963831423, 8.522688052730095348E-16 ) ) ;
#1660 = ADVANCED_FACE ( 'NONE', ( #3667, #697 ), #670, .T. ) ;
#1661 = CARTESIAN_POINT ( 'NONE',  ( 104.0973215944787711, -119.5240462704291389, -1.189271409856590718E-13 ) ) ;
#1662 = CARTESIAN_POINT ( 'NONE',  ( 1.773380156858839873, -67.30899524596459571, -0.8098396333890448551 ) ) ;
#1663 = FACE_OUTER_BOUND ( 'NONE', #1899, .T. ) ;
#1664 = ORIENTED_EDGE ( 'NONE', *, *, #2730, .T. ) ;
#1665 = CARTESIAN_POINT ( 'NONE',  ( 18.21922820888615036, -40.21441497322944514, 3.799573870912058116 ) ) ;
#1666 = CARTESIAN_POINT ( 'NONE',  ( 4.837585924071849952, -61.97584320105620748, 1.412225657785534327 ) ) ;
#1667 = LINE ( 'NONE', #4621, #857 ) ;
#1668 = DIRECTION ( 'NONE',  ( -0.4039838799357113319, -0.9147661038495518149, -9.170600743851232967E-16 ) ) ;
#1669 = EDGE_CURVE ( 'NONE', #6942, #1547, #4737, .T. ) ;
#1670 = ADVANCED_FACE ( 'NONE', ( #5270 ), #5407, .T. ) ;
#1671 = CARTESIAN_POINT ( 'NONE',  ( 1.397902174090916105, -65.57924198930768966, 0.6644065888002452791 ) ) ;
#1672 = CARTESIAN_POINT ( 'NONE',  ( -15.52817266570582611, -38.02681526409561741, -3.000000000000039080 ) ) ;
#1673 = CARTESIAN_POINT ( 'NONE',  ( -4.414126134886927844, -64.86522878795923930, -0.8472126198736709135 ) ) ;
#1674 = ORIENTED_EDGE ( 'NONE', *, *, #5662, .T. ) ;
#1675 = VERTEX_POINT ( 'NONE', #4772 ) ;
#1676 = ORIENTED_EDGE ( 'NONE', *, *, #2776, .T. ) ;
#1677 = AXIS2_PLACEMENT_3D ( 'NONE', #1739, #568, #2134 ) ;
#1678 = LINE ( 'NONE', #3976, #4246 ) ;
#1679 = ORIENTED_EDGE ( 'NONE', *, *, #3432, .F. ) ;
#1680 = FACE_OUTER_BOUND ( 'NONE', #7138, .T. ) ;
#1681 = ADVANCED_FACE ( 'NONE', ( #7059 ), #2390, .F. ) ;
#1682 = EDGE_CURVE ( 'NONE', #5997, #3816, #4700, .T. ) ;
#1683 = CARTESIAN_POINT ( 'NONE',  ( 22.42915535073480982, 21.39736943723329432, -1.493845543551513444 ) ) ;
#1684 = CARTESIAN_POINT ( 'NONE',  ( 5.927764221498110331, -62.35749858221746678, -1.529935281190306862 ) ) ;
#1685 = CARTESIAN_POINT ( 'NONE',  ( -6.519675230953620115, -62.56018929471859735, 1.797154853076760261 ) ) ;
#1686 = VERTEX_POINT ( 'NONE', #3094 ) ;
#1687 = AXIS2_PLACEMENT_3D ( 'NONE', #5281, #2936, #5206 ) ;
#1688 = VERTEX_POINT ( 'NONE', #1277 ) ;
#1689 = CARTESIAN_POINT ( 'NONE',  ( 94.42889356597736139, -103.2882618349535591, -1.027468802220174526E-13 ) ) ;
#1690 = CARTESIAN_POINT ( 'NONE',  ( -3.888488774788935842, -0.9378992740910081505, 3.000000000000000000 ) ) ;
#1691 = CARTESIAN_POINT ( 'NONE',  ( 0.000000000000000000, 0.000000000000000000, -3.500000000000000000 ) ) ;
#1692 = CIRCLE ( 'NONE', #5911, 0.7500000000000000000 ) ;
#1693 = ADVANCED_FACE ( 'NONE', ( #3558 ), #4198, .F. ) ;
#1694 = CARTESIAN_POINT ( 'NONE',  ( -13.76286933773225130, 13.32929763200878881, -0.3999035282155013471 ) ) ;
#1695 = CARTESIAN_POINT ( 'NONE',  ( 13.14859132361180194, 19.41219719266456423, 0.4060579846640096635 ) ) ;
#1696 = CARTESIAN_POINT ( 'NONE',  ( 30.67250997582947747, 4.753907001892506479, -1.499999999999995559 ) ) ;
#1697 = VERTEX_POINT ( 'NONE', #7131 ) ;
#1698 = AXIS2_PLACEMENT_3D ( 'NONE', #3693, #3664, #6012 ) ;
#1699 = ORIENTED_EDGE ( 'NONE', *, *, #3033, .F. ) ;
#1700 = CARTESIAN_POINT ( 'NONE',  ( 18.06097555607235705, -40.30914097186184364, 3.615364355270606289 ) ) ;
#1701 = VECTOR ( 'NONE', #1069, 1000.000000000000000 ) ;
#1702 = DIRECTION ( 'NONE',  ( -0.9721221936972339606, -0.2344748185227520099, 0.000000000000000000 ) ) ;
#1703 = CARTESIAN_POINT ( 'NONE',  ( -20.89962323070193406, -41.21687045383659154, -3.001000000000042078 ) ) ;
#1704 = CARTESIAN_POINT ( 'NONE',  ( -1.855492712959899926, -67.28785520969887557, -0.6321745227666250022 ) ) ;
#1705 = ORIENTED_EDGE ( 'NONE', *, *, #5741, .T. ) ;
#1706 = CARTESIAN_POINT ( 'NONE',  ( -5.107724228862107196, -62.13515610626047447, 3.301466892039410350 ) ) ;
#1707 = AXIS2_PLACEMENT_3D ( 'NONE', #4115, #1266, #3547 ) ;
#1708 = ADVANCED_FACE ( 'NONE', ( #1340 ), #3555, .F. ) ;
#1709 = DIRECTION ( 'NONE',  ( -5.715354789860003484E-18, -9.999836672264337477E-16, 1.000000000000000000 ) ) ;
#1710 = DIRECTION ( 'NONE',  ( -0.9721221936972339606, -0.2344748185227520376, 0.000000000000000000 ) ) ;
#1711 = CARTESIAN_POINT ( 'NONE',  ( -5.408997660349871062, -62.29959681528816873, 3.625047998704080232 ) ) ;
#1712 = CIRCLE ( 'NONE', #3509, 140.0000000000000284 ) ;
#1713 = CARTESIAN_POINT ( 'NONE',  ( 27.65530182349729671, -34.82994948188742512, 3.799124122364484712 ) ) ;
#1714 = FACE_OUTER_BOUND ( 'NONE', #6457, .T. ) ;
#1715 = ORIENTED_EDGE ( 'NONE', *, *, #2768, .F. ) ;
#1716 = ORIENTED_EDGE ( 'NONE', *, *, #6831, .T. ) ;
#1717 = ORIENTED_EDGE ( 'NONE', *, *, #1743, .T. ) ;
#1718 = EDGE_CURVE ( 'NONE', #5680, #3357, #5563, .T. ) ;
#1719 = VECTOR ( 'NONE', #2428, 999.9999999999998863 ) ;
#1720 = VECTOR ( 'NONE', #6644, 1000.000000000000000 ) ;
#1721 = PRODUCT_CONTEXT ( 'NONE', #1264, 'mechanical' ) ;
#1722 = CARTESIAN_POINT ( 'NONE',  ( -43.04083572346265640, -94.50554989113550164, -3.000000000000095479 ) ) ;
#1723 = AXIS2_PLACEMENT_3D ( 'NONE', #2132, #6080, #2708 ) ;
#1724 = ORIENTED_EDGE ( 'NONE', *, *, #3118, .T. ) ;
#1725 = FACE_OUTER_BOUND ( 'NONE', #2424, .T. ) ;
#1726 = DIRECTION ( 'NONE',  ( 0.000000000000000000, 0.000000000000000000, 1.000000000000000000 ) ) ;
#1727 = CARTESIAN_POINT ( 'NONE',  ( 27.11783474234811564, -35.12923323413249221, -1.000000000000034861 ) ) ;
#1728 = CARTESIAN_POINT ( 'NONE',  ( -7.117253929586840222, -62.23044735776716152, 0.7381361199122749017 ) ) ;
#1729 = VECTOR ( 'NONE', #6046, 1000.000000000000227 ) ;
#1730 = VECTOR ( 'NONE', #4636, 1000.000000000000000 ) ;
#1731 = ORIENTED_EDGE ( 'NONE', *, *, #6011, .F. ) ;
#1732 = ORIENTED_EDGE ( 'NONE', *, *, #5730, .T. ) ;
#1733 = EDGE_CURVE ( 'NONE', #5350, #6877, #627, .T. ) ;
#1734 = AXIS2_PLACEMENT_3D ( 'NONE', #3431, #2261, #3918 ) ;
#1735 = DIRECTION ( 'NONE',  ( -0.9721221936972339606, -0.2344748185227520099, 0.000000000000000000 ) ) ;
#1736 = LINE ( 'NONE', #2219, #6315 ) ;
#1737 = AXIS2_PLACEMENT_3D ( 'NONE', #5345, #3726, #2030 ) ;
#1738 = FACE_OUTER_BOUND ( 'NONE', #6531, .T. ) ;
#1739 = CARTESIAN_POINT ( 'NONE',  ( 104.0973215944787711, -119.5240462704291389, -3.000000000000119904 ) ) ;
#1740 = DIRECTION ( 'NONE',  ( -0.9879743132267128081, -0.1546180985661290141, -1.602621969470799848E-16 ) ) ;
#1741 = EDGE_LOOP ( 'NONE', ( #2241, #2822, #2285, #6053 ) ) ;
#1742 = VERTEX_POINT ( 'NONE', #2722 ) ;
#1743 = EDGE_CURVE ( 'NONE', #3341, #5578, #2426, .T. ) ;
#1744 = AXIS2_PLACEMENT_3D ( 'NONE', #762, #1916, #4877 ) ;
#1745 = CARTESIAN_POINT ( 'NONE',  ( -11.40395268922818062, 1.749910050107414738, 1.734723475976807094E-15 ) ) ;
#1746 = CYLINDRICAL_SURFACE ( 'NONE', #4980, 5.000000000000000000 ) ;
#1747 = DIRECTION ( 'NONE',  ( -0.1628827478269146978, 0.7884342920379695530, -0.5931615105508275532 ) ) ;
#1748 = CARTESIAN_POINT ( 'NONE',  ( 5.975049724055580214, -64.37929422792591083, -2.133092136665421190 ) ) ;
#1749 = LINE ( 'NONE', #4045, #1846 ) ;
#1750 = VERTEX_POINT ( 'NONE', #954 ) ;
#1751 = DIRECTION ( 'NONE',  ( 0.9492899500389728740, 0.3144019573014844582, 0.000000000000000000 ) ) ;
#1752 = DIRECTION ( 'NONE',  ( -5.715354789860003484E-18, -9.999836672264337477E-16, 1.000000000000000000 ) ) ;
#1753 = CARTESIAN_POINT ( 'NONE',  ( -4.860610968486169803, -1.172374092613760022, -3.500000000000000000 ) ) ;
#1754 = LINE ( 'NONE', #4080, #1365 ) ;
#1755 = CARTESIAN_POINT ( 'NONE',  ( 5.010558598472139913, -57.30068827582834956, 0.4001341763009204078 ) ) ;
#1756 = CARTESIAN_POINT ( 'NONE',  ( 26.98470030103655404, -34.62962642788639300, 3.486735179637458604 ) ) ;
#1757 = DIRECTION ( 'NONE',  ( 0.000000000000000000, -0.7252570966694442678, 0.6884781359858920258 ) ) ;
#1758 = VERTEX_POINT ( 'NONE', #834 ) ;
#1759 = ORIENTED_EDGE ( 'NONE', *, *, #5, .T. ) ;
#1760 = ORIENTED_EDGE ( 'NONE', *, *, #1281, .F. ) ;
#1761 = PRODUCT_DEFINITION_SHAPE ( 'NONE', 'NONE',  #7446 ) ;
#1762 = LINE ( 'NONE', #5760, #642 ) ;
#1763 = CARTESIAN_POINT ( 'NONE',  ( 7.529070345495034289, 16.11642554373085900, 3.000000000000015987 ) ) ;
#1764 = CARTESIAN_POINT ( 'NONE',  ( -3.760984799052800476, -54.43314106586858969, -1.957528877657078059 ) ) ;
#1765 = LINE ( 'NONE', #1127, #5714 ) ;
#1766 = CARTESIAN_POINT ( 'NONE',  ( -1.503553670228684913, -55.21328561235763743, -1.985649781529471802 ) ) ;
#1767 = EDGE_CURVE ( 'NONE', #5892, #4812, #3131, .T. ) ;
#1768 = ORIENTED_EDGE ( 'NONE', *, *, #393, .F. ) ;
#1769 = ORIENTED_EDGE ( 'NONE', *, *, #1400, .F. ) ;
#1770 = CARTESIAN_POINT ( 'NONE',  ( 41.70778007397900211, -94.98992620957551480, -9.454242944073598665E-14 ) ) ;
#1771 = DIRECTION ( 'NONE',  ( -0.4039838799357104437, -0.9147661038495520369, -1.600849619044994772E-16 ) ) ;
#1772 = CARTESIAN_POINT ( 'NONE',  ( -14.70408710852078116, -35.66654345889202204, -3.000000000000036415 ) ) ;
#1773 = DIRECTION ( 'NONE',  ( -5.715354789860003484E-18, -9.999836672264337477E-16, 1.000000000000000000 ) ) ;
#1774 = EDGE_CURVE ( 'NONE', #3729, #3069, #3776, .T. ) ;
#1775 = EDGE_CURVE ( 'NONE', #4598, #1742, #4955, .T. ) ;
#1776 = CARTESIAN_POINT ( 'NONE',  ( 26.67188031194815068, 24.16129507000589527, -2.993845543551515664 ) ) ;
#1777 = ORIENTED_EDGE ( 'NONE', *, *, #1281, .T. ) ;
#1778 = DIRECTION ( 'NONE',  ( 5.715354789845004342E-18, 9.999836672264337477E-16, -1.000000000000000000 ) ) ;
#1779 = CARTESIAN_POINT ( 'NONE',  ( 43.95483829995806957, -94.87490738911687060, 2.999999999999905409 ) ) ;
#1780 = EDGE_CURVE ( 'NONE', #4731, #6736, #6713, .T. ) ;
#1781 = CARTESIAN_POINT ( 'NONE',  ( -4.718809332073220730, -63.89081786388664597, 1.455152677735624289 ) ) ;
#1782 = CARTESIAN_POINT ( 'NONE',  ( 3.942295684294244928, -66.34053734621645049, -3.017350621022677259 ) ) ;
#1783 = DIRECTION ( 'NONE',  ( 0.9793199139485100346, 0.2023178344681531293, 1.787644449902631965E-16 ) ) ;
#1784 = ORIENTED_EDGE ( 'NONE', *, *, #2131, .T. ) ;
#1785 = CARTESIAN_POINT ( 'NONE',  ( -4.949227490188758516, -62.08336044754862826, 3.140672163054920585 ) ) ;
#1786 = DIRECTION ( 'NONE',  ( -0.1546180985661130547, 0.9879743132267154726, 9.870744795757317374E-16 ) ) ;
#1787 = DIRECTION ( 'NONE',  ( -0.8039121061460989814, 0.3550279469270786747, -0.4771587602596088495 ) ) ;
#1788 = ADVANCED_FACE ( 'NONE', ( #2148 ), #3246, .F. ) ;
#1789 = CARTESIAN_POINT ( 'NONE',  ( 4.977719985769329725, -63.63849604921595216, 2.874328699340139792 ) ) ;
#1790 = CARTESIAN_POINT ( 'NONE',  ( -1.592557218785495055, -66.68601476236933934, 1.076257986235874764 ) ) ;
#1791 = DIRECTION ( 'NONE',  ( 0.9492899500389719858, 0.3144019573014870117, 0.000000000000000000 ) ) ;
#1792 = ORIENTED_EDGE ( 'NONE', *, *, #2970, .T. ) ;
#1793 = EDGE_LOOP ( 'NONE', ( #2145, #2982, #3445, #1406, #538, #4127 ) ) ;
#1794 = ORIENTED_EDGE ( 'NONE', *, *, #5679, .T. ) ;
#1795 = CARTESIAN_POINT ( 'NONE',  ( 11.65361085287446663, 10.55667343862480223, 3.000000000000010658 ) ) ;
#1796 = CARTESIAN_POINT ( 'NONE',  ( 28.12455780688322449, -37.01391159201033787, -3.686287386450715076E-14 ) ) ;
#1797 = CARTESIAN_POINT ( 'NONE',  ( -5.707180516281660232, -57.33854382299282548, -2.489482313002657321 ) ) ;
#1798 = CARTESIAN_POINT ( 'NONE',  ( 27.65480120734329006, -34.83022826066387267, -0.7995651912284664764 ) ) ;
#1799 = ORIENTED_EDGE ( 'NONE', *, *, #3271, .T. ) ;
#1800 = AXIS2_PLACEMENT_3D ( 'NONE', #4906, #1425, #6085 ) ;
#1801 = EDGE_CURVE ( 'NONE', #553, #5128, #5448, .T. ) ;
#1802 = DIRECTION ( 'NONE',  ( 5.715354789860003484E-18, 9.999836672264337477E-16, -1.000000000000000000 ) ) ;
#1803 = ADVANCED_BREP_SHAPE_REPRESENTATION ( '', ( #2394, #751 ), #989 ) ;
#1804 = CARTESIAN_POINT ( 'NONE',  ( 22.42915535073480982, 21.39736943723329432, -1.493845543551513444 ) ) ;
#1805 = AXIS2_PLACEMENT_3D ( 'NONE', #7039, #5280, #82 ) ;
#1806 = CARTESIAN_POINT ( 'NONE',  ( -9.311346830843410416, -51.41373841511900622, 1.033728595105000148 ) ) ;
#1807 = DIRECTION ( 'NONE',  ( 0.9793199139485101457, 0.2023178344681531016, 2.079116908177651894E-16 ) ) ;
#1808 = CARTESIAN_POINT ( 'NONE',  ( 14.63724902514210058, -36.05867701049984930, 4.346656902870709160 ) ) ;
#1809 = VECTOR ( 'NONE', #1622, 1000.000000000000000 ) ;
#1810 = EDGE_CURVE ( 'NONE', #184, #5945, #3298, .T. ) ;
#1811 = CARTESIAN_POINT ( 'NONE',  ( -2.603817572988885054, -64.79915130424556935, -0.08835382460255962467 ) ) ;
#1812 = LINE ( 'NONE', #5254, #6845 ) ;
#1813 = CARTESIAN_POINT ( 'NONE',  ( 5.440311866380434402, -58.19481930409472881, 0.4849701219046175238 ) ) ;
#1814 = CIRCLE ( 'NONE', #2647, 0.7500000000000002220 ) ;
#1815 = FACE_OUTER_BOUND ( 'NONE', #1187, .T. ) ;
#1816 = ORIENTED_EDGE ( 'NONE', *, *, #3604, .T. ) ;
#1817 = DIRECTION ( 'NONE',  ( 0.4039838799357100552, 0.9147661038495522590, 1.399039571475124858E-16 ) ) ;
#1818 = EDGE_CURVE ( 'NONE', #2009, #6491, #1006, .T. ) ;
#1819 = EDGE_CURVE ( 'NONE', #1942, #3815, #6056, .T. ) ;
#1820 = LINE ( 'NONE', #4760, #1253 ) ;
#1821 = CARTESIAN_POINT ( 'NONE',  ( -2.909477865675369923, -55.29415281518058833, 1.990524098341705406 ) ) ;
#1822 = CARTESIAN_POINT ( 'NONE',  ( -3.569041007005829602, -65.81017109676685095, 3.284668648760890264 ) ) ;
#1823 = DIRECTION ( 'NONE',  ( 0.9793199139485101457, 0.2023178344681531016, 2.079116908177651894E-16 ) ) ;
#1824 = ORIENTED_EDGE ( 'NONE', *, *, #5459, .T. ) ;
#1825 = ORIENTED_EDGE ( 'NONE', *, *, #7183, .F. ) ;
#1826 = VERTEX_POINT ( 'NONE', #396 ) ;
#1827 = ORIENTED_EDGE ( 'NONE', *, *, #1427, .T. ) ;
#1828 = DIRECTION ( 'NONE',  ( 0.7411265327553895332, 0.6713653717953992350, 6.755902076156662974E-16 ) ) ;
#1829 = AXIS2_PLACEMENT_3D ( 'NONE', #3249, #4316, #6605 ) ;
#1830 = CARTESIAN_POINT ( 'NONE',  ( 7.529070345495034289, 16.11642554373086256, 1.604619215278546562E-14 ) ) ;
#1831 = CARTESIAN_POINT ( 'NONE',  ( -1.432436674628349893, -67.38906872584260555, -2.752582849501530760 ) ) ;
#1832 = FACE_OUTER_BOUND ( 'NONE', #611, .T. ) ;
#1833 = STYLED_ITEM ( 'NONE', ( #4522 ), #2417 ) ;
#1834 = ORIENTED_EDGE ( 'NONE', *, *, #2768, .T. ) ;
#1835 = CIRCLE ( 'NONE', #2432, 2.999999999999999556 ) ;
#1836 = PLANE ( 'NONE',  #40 ) ;
#1837 = VECTOR ( 'NONE', #5194, 1000.000000000000114 ) ;
#1838 = CARTESIAN_POINT ( 'NONE',  ( -11.40395268922818062, 1.749910050107411630, 3.000000000000001776 ) ) ;
#1839 = CIRCLE ( 'NONE', #4008, 2.249999999999962252 ) ;
#1840 = CYLINDRICAL_SURFACE ( 'NONE', #4375, 147.0000000000000284 ) ;
#1841 = DIRECTION ( 'NONE',  ( -0.9999836672264332815, 0.005715354789842956411, 0.000000000000000000 ) ) ;
#1842 = CARTESIAN_POINT ( 'NONE',  ( 0.4291165664073187114, -54.21109657073610322, 2.063524181601441132 ) ) ;
#1843 = AXIS2_PLACEMENT_3D ( 'NONE', #4436, #1726, #6839 ) ;
#1844 = AXIS2_PLACEMENT_3D ( 'NONE', #2492, #166, #1370 ) ;
#1845 = CARTESIAN_POINT ( 'NONE',  ( 2.818173014649640429, -55.92969527921476924, 1.989760685886134972 ) ) ;
#1846 = VECTOR ( 'NONE', #6346, 1000.000000000000000 ) ;
#1847 = AXIS2_PLACEMENT_3D ( 'NONE', #7148, #227, #2518 ) ;
#1848 = DIRECTION ( 'NONE',  ( -0.3144066910790611624, -0.9492883822130743221, 0.000000000000000000 ) ) ;
#1849 = CARTESIAN_POINT ( 'NONE',  ( 1.814912623942119829, -54.89591502488989505, 0.1965585422507683810 ) ) ;
#1850 = CARTESIAN_POINT ( 'NONE',  ( -3.365275581743949918, -66.00192919971716776, -0.8990674732841750227 ) ) ;
#1851 = ADVANCED_FACE ( 'NONE', ( #881, #4393 ), #4886, .T. ) ;
#1852 = DIRECTION ( 'NONE',  ( 0.2098925886716649092, 0.9716434517700405227, -0.1088765532752961201 ) ) ;
#1853 = AXIS2_PLACEMENT_3D ( 'NONE', #678, #5914, #108 ) ;
#1854 = ORIENTED_EDGE ( 'NONE', *, *, #6843, .F. ) ;
#1855 = CARTESIAN_POINT ( 'NONE',  ( 39.32685927492619982, -94.35036853610694152, 2.999999999999905853 ) ) ;
#1856 = CIRCLE ( 'NONE', #4149, 0.9999999999999998890 ) ;
#1857 = CARTESIAN_POINT ( 'NONE',  ( -7.741417275248890562, 12.33509147838778830, 1.214306433183764966E-14 ) ) ;
#1858 = CARTESIAN_POINT ( 'NONE',  ( 4.492111197601039052, 14.38610368760445546, 1.431146867680865853E-14 ) ) ;
#1859 = CARTESIAN_POINT ( 'NONE',  ( 1.711268714270854918, -65.48362256684714566, -1.456162841279315945 ) ) ;
#1860 = CARTESIAN_POINT ( 'NONE',  ( -1.974098099753330171, -66.57628266072889289, 3.196874607719439876 ) ) ;
#1861 = DIRECTION ( 'NONE',  ( -5.715354789860003484E-18, -9.999836672264337477E-16, 1.000000000000000000 ) ) ;
#1862 = EDGE_CURVE ( 'NONE', #1005, #5988, #1254, .T. ) ;
#1863 = EDGE_LOOP ( 'NONE', ( #1161, #6234, #3613, #4229 ) ) ;
#1864 = ORIENTED_EDGE ( 'NONE', *, *, #6450, .T. ) ;
#1865 = VERTEX_POINT ( 'NONE', #2114 ) ;
#1866 = DIRECTION ( 'NONE',  ( 0.000000000000000000, 0.000000000000000000, -1.000000000000000000 ) ) ;
#1867 = CARTESIAN_POINT ( 'NONE',  ( -16.21021049057420882, 1.692961427013494724, -2.993845543551527655 ) ) ;
#1868 = CARTESIAN_POINT ( 'NONE',  ( -6.776085205154060986, -62.52991726716069820, -2.400146893717961749 ) ) ;
#1869 = CARTESIAN_POINT ( 'NONE',  ( 4.860610968486169803, 1.172374092613760688, -3.500000000000000000 ) ) ;
#1870 = EDGE_CURVE ( 'NONE', #1742, #6678, #4838, .T. ) ;
#1871 = ORIENTED_EDGE ( 'NONE', *, *, #3864, .F. ) ;
#1872 = ORIENTED_EDGE ( 'NONE', *, *, #1260, .T. ) ;
#1873 = FACE_OUTER_BOUND ( 'NONE', #5304, .T. ) ;
#1874 = DIRECTION ( 'NONE',  ( -5.715354789845005112E-18, -9.999836672264339449E-16, 1.000000000000000000 ) ) ;
#1875 = DIRECTION ( 'NONE',  ( -0.4328040977884316520, 0.5819352847797604200, 0.6884997728872834788 ) ) ;
#1876 = CARTESIAN_POINT ( 'NONE',  ( -5.206993624623629913, -63.95781028998001716, 3.417603084305509853 ) ) ;
#1877 = CARTESIAN_POINT ( 'NONE',  ( 15.94457129749017277, -41.07922723232461237, 2.999999999999958700 ) ) ;
#1878 = CARTESIAN_POINT ( 'NONE',  ( -5.710866809226770258, -58.90547762198222870, 1.725351541085619500 ) ) ;
#1879 = CARTESIAN_POINT ( 'NONE',  ( -10.26063678088237907, -51.72814037242050489, 2.533728595105000370 ) ) ;
#1880 = DIRECTION ( 'NONE',  ( -5.715354789845005112E-18, -9.999836672264339449E-16, 1.000000000000000000 ) ) ;
#1881 = CARTESIAN_POINT ( 'NONE',  ( -1.847236269850647705, -65.97879705718997911, -0.8523026458531161031 ) ) ;
#1882 = ORIENTED_EDGE ( 'NONE', *, *, #491, .T. ) ;
#1883 = CARTESIAN_POINT ( 'NONE',  ( -14.97059744062764075, -34.32647288175419931, -2.566271404895000163 ) ) ;
#1884 = ADVANCED_FACE ( 'NONE', ( #356 ), #2648, .T. ) ;
#1885 = CYLINDRICAL_SURFACE ( 'NONE', #2212, 0.5000000000000004441 ) ;
#1886 = CARTESIAN_POINT ( 'NONE',  ( 17.61082888335783991, -39.97043405836763696, -0.1337947118489001552 ) ) ;
#1887 = CARTESIAN_POINT ( 'NONE',  ( 3.660823140336725068, -65.74644859602665292, -1.309095517728299907 ) ) ;
#1888 = CARTESIAN_POINT ( 'NONE',  ( -4.574768583212910578, -63.39215034952142247, -2.605000795493774834 ) ) ;
#1889 = CARTESIAN_POINT ( 'NONE',  ( 7.283874945971848369, -8.906884184084097100, -8.865108780400335494E-15 ) ) ;
#1890 = DIRECTION ( 'NONE',  ( -0.08966155106958693943, -0.9959722919136836383, 0.000000000000000000 ) ) ;
#1891 = ORIENTED_EDGE ( 'NONE', *, *, #2536, .T. ) ;
#1892 = EDGE_LOOP ( 'NONE', ( #1794, #5333, #4085, #5003 ) ) ;
#1893 = VERTEX_POINT ( 'NONE', #3399 ) ;
#1894 = DIRECTION ( 'NONE',  ( -5.715354789860003484E-18, -9.999836672264337477E-16, 1.000000000000000000 ) ) ;
#1895 = FACE_BOUND ( 'NONE', #2242, .T. ) ;
#1896 = CARTESIAN_POINT ( 'NONE',  ( 5.742131165818880056, -64.29439030986208081, -3.151051222873450630 ) ) ;
#1897 = CARTESIAN_POINT ( 'NONE',  ( 5.927764221498110331, -62.35749858221746678, -1.529935281190306862 ) ) ;
#1898 = ORIENTED_EDGE ( 'NONE', *, *, #3686, .F. ) ;
#1899 = EDGE_LOOP ( 'NONE', ( #657, #4674, #251, #1937 ) ) ;
#1900 = EDGE_CURVE ( 'NONE', #4244, #6025, #7130, .T. ) ;
#1901 = EDGE_CURVE ( 'NONE', #3586, #5496, #6981, .T. ) ;
#1902 = DIRECTION ( 'NONE',  ( 0.1200071523045019850, -0.5808948794702039065, -0.8050834878452428622 ) ) ;
#1903 = SPHERICAL_SURFACE ( 'NONE', #1853, 7.844444444444450326 ) ;
#1904 = DIRECTION ( 'NONE',  ( -0.4039838799357163279, -0.9147661038495494834, -8.673617379884193244E-16 ) ) ;
#1905 = CARTESIAN_POINT ( 'NONE',  ( -40.82267254781529431, -94.88271315313488685, -3.000000000000095923 ) ) ;
#1906 = VERTEX_POINT ( 'NONE', #5673 ) ;
#1907 = VECTOR ( 'NONE', #7151, 999.9999999999998863 ) ;
#1908 = CARTESIAN_POINT ( 'NONE',  ( 5.113035703684060351, -58.96629286118465529, 0.1341944340671852032 ) ) ;
#1909 = AXIS2_PLACEMENT_3D ( 'NONE', #6047, #2460, #315 ) ;
#1910 = CARTESIAN_POINT ( 'NONE',  ( 14.63763862841555330, 20.11382921380837629, 0.006154456448490084469 ) ) ;
#1911 = CARTESIAN_POINT ( 'NONE',  ( -16.40387102536037744, 1.778486824056639826, 1.734723475976807094E-15 ) ) ;
#1912 = CARTESIAN_POINT ( 'NONE',  ( 0.01932788389254917402, -54.65463053036518914, 0.09165168851670162098 ) ) ;
#1913 = STYLED_ITEM ( 'NONE', ( #4650 ), #4713 ) ;
#1914 = VERTEX_POINT ( 'NONE', #6912 ) ;
#1915 = FACE_OUTER_BOUND ( 'NONE', #5311, .T. ) ;
#1916 = DIRECTION ( 'NONE',  ( -5.715354789845005112E-18, -9.999836672264339449E-16, 1.000000000000000000 ) ) ;
#1917 = FACE_OUTER_BOUND ( 'NONE', #3479, .T. ) ;
#1918 = CARTESIAN_POINT ( 'NONE',  ( 0.000000000000000000, 0.000000000000000000, -3.000000000000000000 ) ) ;
#1919 = CARTESIAN_POINT ( 'NONE',  ( 3.403992074353090036, -54.97443010399496899, 2.224669212202579960 ) ) ;
#1920 = DIRECTION ( 'NONE',  ( -0.9999836672264335036, 0.005715354789845003385, 1.110223024625156047E-16 ) ) ;
#1921 = ORIENTED_EDGE ( 'NONE', *, *, #112, .F. ) ;
#1922 = VERTEX_POINT ( 'NONE', #2353 ) ;
#1923 = AXIS2_PLACEMENT_3D ( 'NONE', #5526, #351, #1336 ) ;
#1924 = DIRECTION ( 'NONE',  ( 0.9999836672264331705, -0.005715354789859876036, 0.000000000000000000 ) ) ;
#1925 = LINE ( 'NONE', #5300, #7241 ) ;
#1926 = CARTESIAN_POINT ( 'NONE',  ( -2.876828494605734754, -55.82398600891924190, -2.074803592940099861 ) ) ;
#1927 = ORIENTED_EDGE ( 'NONE', *, *, #4263, .F. ) ;
#1928 = EDGE_CURVE ( 'NONE', #4359, #427, #1667, .T. ) ;
#1929 = ORIENTED_EDGE ( 'NONE', *, *, #6393, .F. ) ;
#1930 = VERTEX_POINT ( 'NONE', #548 ) ;
#1931 = AXIS2_PLACEMENT_3D ( 'NONE', #1036, #2750, #7347 ) ;
#1932 = AXIS2_PLACEMENT_3D ( 'NONE', #5358, #2482, #3176 ) ;
#1933 = DIRECTION ( 'NONE',  ( 0.9793199139485100346, 0.2023178344681531293, 1.804112415015879378E-16 ) ) ;
#1934 = DIRECTION ( 'NONE',  ( -5.715354789845005112E-18, -9.999836672264339449E-16, 1.000000000000000000 ) ) ;
#1935 = DIRECTION ( 'NONE',  ( 0.4364886600403651840, -0.1927644473149899840, -0.8788171126619650497 ) ) ;
#1936 = CARTESIAN_POINT ( 'NONE',  ( -2.148471732745839802, -67.07461398899560834, 3.078016402823839925 ) ) ;
#1937 = ORIENTED_EDGE ( 'NONE', *, *, #892, .T. ) ;
#1938 = TOROIDAL_SURFACE ( 'NONE', #4608, 1.500000000000000000, 1.000000000000000000 ) ;
#1939 = EDGE_CURVE ( 'NONE', #5128, #320, #5787, .T. ) ;
#1940 = EDGE_CURVE ( 'NONE', #5032, #4548, #3322, .T. ) ;
#1941 = CIRCLE ( 'NONE', #3870, 1.000000000000000444 ) ;
#1942 = VERTEX_POINT ( 'NONE', #6205 ) ;
#1943 = DIRECTION ( 'NONE',  ( 0.2223191033124283789, 0.6712482523644727195, 0.7071067811865466846 ) ) ;
#1944 = CIRCLE ( 'NONE', #5579, 6.299999999999998934 ) ;
#1945 = CARTESIAN_POINT ( 'NONE',  ( 1.570963842414029976, -66.14661321919228953, 1.018783762524700265 ) ) ;
#1946 = AXIS2_PLACEMENT_3D ( 'NONE', #4177, #5960, #780 ) ;
#1947 = CYLINDRICAL_SURFACE ( 'NONE', #4726, 0.9999999999999991118 ) ;
#1948 = CARTESIAN_POINT ( 'NONE',  ( -34.88460058024262622, 16.28046363954885933, -2.243845543551999722 ) ) ;
#1949 = CARTESIAN_POINT ( 'NONE',  ( 5.168836016896262819, -63.16969723543360260, -3.422093515887588477 ) ) ;
#1950 = VECTOR ( 'NONE', #3402, 1000.000000000000000 ) ;
#1951 = EDGE_CURVE ( 'NONE', #7317, #3224, #3925, .T. ) ;
#1952 = AXIS2_PLACEMENT_3D ( 'NONE', #7203, #4349, #6637 ) ;
#1953 = ORIENTED_EDGE ( 'NONE', *, *, #1587, .T. ) ;
#1954 = CIRCLE ( 'NONE', #3162, 1.000000000000000888 ) ;
#1955 = CARTESIAN_POINT ( 'NONE',  ( 14.63763862841553376, 20.11382921380832656, 0.006154456448485313980 ) ) ;
#1956 = TOROIDAL_SURFACE ( 'NONE', #2928, 1.500000000000000000, 1.000000000000000000 ) ;
#1957 = CARTESIAN_POINT ( 'NONE',  ( 41.70778007397900211, -94.98992620957551480, -1.000000000000094591 ) ) ;
#1958 = CARTESIAN_POINT ( 'NONE',  ( 18.74668230531429458, -39.89873697698326538, -1.000000000000039746 ) ) ;
#1959 = CARTESIAN_POINT ( 'NONE',  ( -6.129265975028279634, -62.42766041111902098, -0.6909925287373350766 ) ) ;
#1960 = VECTOR ( 'NONE', #389, 1000.000000000000000 ) ;
#1961 = CARTESIAN_POINT ( 'NONE',  ( -4.101849953070630050, -66.53066707031882743, 2.593177719986650143 ) ) ;
#1962 = DIRECTION ( 'NONE',  ( -1.046706025223848628E-16, 1.111638688234981601E-15, -1.000000000000000000 ) ) ;
#1963 = EDGE_CURVE ( 'NONE', #3938, #4894, #6275, .T. ) ;
#1964 = ORIENTED_EDGE ( 'NONE', *, *, #6706, .T. ) ;
#1965 = ORIENTED_EDGE ( 'NONE', *, *, #5377, .F. ) ;
#1966 = AXIS2_PLACEMENT_3D ( 'NONE', #6502, #2993, #143 ) ;
#1967 = CARTESIAN_POINT ( 'NONE',  ( 4.860610968486169803, 1.172374092613760688, 3.500000000000000000 ) ) ;
#1968 = CARTESIAN_POINT ( 'NONE',  ( 43.95483829995806957, -94.87490738911687060, -9.454242944073598665E-14 ) ) ;
#1969 = CARTESIAN_POINT ( 'NONE',  ( -2.527830428429834964, -65.26309079616396502, -2.780623214462280668 ) ) ;
#1970 = CARTESIAN_POINT ( 'NONE',  ( 4.443182564071356033, -64.83719503748011448, 0.7261340252908324855 ) ) ;
#1971 = ORIENTED_EDGE ( 'NONE', *, *, #4294, .T. ) ;
#1972 = VERTEX_POINT ( 'NONE', #510 ) ;
#1973 = VERTEX_POINT ( 'NONE', #1753 ) ;
#1974 = EDGE_LOOP ( 'NONE', ( #4471, #7057, #3330, #5758 ) ) ;
#1975 = APPLICATION_PROTOCOL_DEFINITION ( 'draft international standard', 'automotive_design', 1998, #2544 ) ;
#1976 = FACE_OUTER_BOUND ( 'NONE', #4311, .T. ) ;
#1977 = EDGE_CURVE ( 'NONE', #3563, #3666, #4230, .T. ) ;
#1978 = DIRECTION ( 'NONE',  ( 0.1860016876085203719, -0.1636620475539280195, 0.9688230521603200529 ) ) ;
#1979 = FACE_OUTER_BOUND ( 'NONE', #6015, .T. ) ;
#1980 = CARTESIAN_POINT ( 'NONE',  ( 6.802585521241110378, -58.92636561181245014, 2.370308086683080351 ) ) ;
#1981 = ORIENTED_EDGE ( 'NONE', *, *, #345, .F. ) ;
#1982 = EDGE_LOOP ( 'NONE', ( #4442, #7291, #4991, #554 ) ) ;
#1983 = ORIENTED_EDGE ( 'NONE', *, *, #5090, .T. ) ;
#1984 = CARTESIAN_POINT ( 'NONE',  ( -105.7473861751082040, -118.0666774205683822, -1.000000000000118794 ) ) ;
#1985 = CARTESIAN_POINT ( 'NONE',  ( 5.755397240816559901, -61.80640411027656000, 0.6650717595513898628 ) ) ;
#1986 = EDGE_CURVE ( 'NONE', #4548, #2317, #2565, .T. ) ;
#1987 = PLANE ( 'NONE',  #3022 ) ;
#1988 = EDGE_CURVE ( 'NONE', #6323, #4962, #4721, .T. ) ;
#1989 = DIRECTION ( 'NONE',  ( 0.9492899500389723189, 0.3144019573014865121, 0.000000000000000000 ) ) ;
#1990 = CARTESIAN_POINT ( 'NONE',  ( -4.048469865975810933, -56.30416671985942401, -2.268338689207286318 ) ) ;
#1991 = PRODUCT_DEFINITION_SHAPE ( 'NONE', 'NONE',  #1226 ) ;
#1992 = VERTEX_POINT ( 'NONE', #5110 ) ;
#1993 = DIRECTION ( 'NONE',  ( -0.9828140593167949968, 0.1845982795403122156, 4.010227384219995304E-16 ) ) ;
#1994 = EDGE_CURVE ( 'NONE', #5010, #4166, #4480, .T. ) ;
#1995 = DIRECTION ( 'NONE',  ( -0.5224671166576538850, 0.8526594349512809368, 0.000000000000000000 ) ) ;
#1996 = ADVANCED_FACE ( 'NONE', ( #7391 ), #1635, .T. ) ;
#1997 = CARTESIAN_POINT ( 'NONE',  ( 39.48483786921892857, -95.33781693134928048, 2.999999999999904965 ) ) ;
#1998 = CARTESIAN_POINT ( 'NONE',  ( 2.080482015124565098, -66.54183146390657555, -1.221303033644861813 ) ) ;
#1999 = CARTESIAN_POINT ( 'NONE',  ( -6.955550688080649913, -62.00810176775132021, 2.849210506046880642 ) ) ;
#2000 = FACE_OUTER_BOUND ( 'NONE', #4206, .T. ) ;
#2001 = EDGE_LOOP ( 'NONE', ( #5157, #1521, #1295, #1537 ) ) ;
#2002 = ORIENTED_EDGE ( 'NONE', *, *, #4197, .F. ) ;
#2003 = EDGE_LOOP ( 'NONE', ( #1531, #353, #666, #7297 ) ) ;
#2004 = DIRECTION ( 'NONE',  ( 5.715354789860003484E-18, 9.999836672264337477E-16, -1.000000000000000000 ) ) ;
#2005 = DIRECTION ( 'NONE',  ( 0.000000000000000000, 0.000000000000000000, -1.000000000000000000 ) ) ;
#2006 = CARTESIAN_POINT ( 'NONE',  ( 1.276103242900551882, -55.15251840166065733, -1.809563881513800876 ) ) ;
#2007 = DIRECTION ( 'NONE',  ( -5.715354789860003484E-18, -9.999836672264337477E-16, 1.000000000000000000 ) ) ;
#2008 = CARTESIAN_POINT ( 'NONE',  ( -5.524031959655990143, -63.36203416574449676, 3.453224700803013025 ) ) ;
#2009 = VERTEX_POINT ( 'NONE', #471 ) ;
#2010 = ORIENTED_EDGE ( 'NONE', *, *, #5795, .T. ) ;
#2011 = PRODUCT_CONTEXT ( 'NONE', #4578, 'mechanical' ) ;
#2012 = CARTESIAN_POINT ( 'NONE',  ( 14.02750760687355935, -37.17441268192290238, 0.4975185951050001831 ) ) ;
#2013 = DIRECTION ( 'NONE',  ( 0.000000000000000000, 0.000000000000000000, -1.000000000000000000 ) ) ;
#2014 = FACE_OUTER_BOUND ( 'NONE', #4851, .T. ) ;
#2015 = CARTESIAN_POINT ( 'NONE',  ( 1.530679711083600125, -53.64394877353957014, -0.1027361406249600040 ) ) ;
#2016 = ORIENTED_EDGE ( 'NONE', *, *, #1182, .T. ) ;
#2017 = EDGE_CURVE ( 'NONE', #1697, #7442, #4501, .T. ) ;
#2018 = CARTESIAN_POINT ( 'NONE',  ( -28.70619392989860330, -36.67182071578998404, -3.683528784622187242E-14 ) ) ;
#2019 = CARTESIAN_POINT ( 'NONE',  ( 4.348279337280104961, -63.27746244242579365, -1.677170969482009832 ) ) ;
#2020 = VERTEX_POINT ( 'NONE', #1110 ) ;
#2021 = CIRCLE ( 'NONE', #7319, 140.0000000000000284 ) ;
#2022 = LINE ( 'NONE', #2103, #823 ) ;
#2023 = DIRECTION ( 'NONE',  ( 0.3128463504745289669, 0.9445772445362837777, 0.09950371902099817978 ) ) ;
#2024 = ORIENTED_EDGE ( 'NONE', *, *, #419, .T. ) ;
#2025 = CIRCLE ( 'NONE', #1090, 140.0000000000000000 ) ;
#2026 = CARTESIAN_POINT ( 'NONE',  ( -28.26642576027046516, -36.90973657692984489, -3.000000000000037748 ) ) ;
#2027 = CARTESIAN_POINT ( 'NONE',  ( -7.741417275248890562, 12.33509147838778830, 1.214306433183764966E-14 ) ) ;
#2028 = CARTESIAN_POINT ( 'NONE',  ( -12.11759654540111875, 13.15705282150456590, 3.000000000000012879 ) ) ;
#2029 = DIRECTION ( 'NONE',  ( -0.2023178344681530183, 0.9793199139485100346, 8.673617379884158732E-16 ) ) ;
#2030 = DIRECTION ( 'NONE',  ( 5.715354789845005112E-18, 9.999836672264339449E-16, -1.000000000000000000 ) ) ;
#2031 = AXIS2_PLACEMENT_3D ( 'NONE', #6933, #5812, #2481 ) ;
#2032 = CARTESIAN_POINT ( 'NONE',  ( -6.722550792682009835, -58.60332661353002948, 1.487589938850535143 ) ) ;
#2033 = CARTESIAN_POINT ( 'NONE',  ( 9.327049558211379932, -51.36650955289220377, -1.499999999999997780 ) ) ;
#2034 = ORIENTED_EDGE ( 'NONE', *, *, #802, .F. ) ;
#2035 = EDGE_CURVE ( 'NONE', #4040, #7181, #1238, .T. ) ;
#2036 = EDGE_CURVE ( 'NONE', #420, #7068, #3939, .T. ) ;
#2037 = ORIENTED_EDGE ( 'NONE', *, *, #6968, .T. ) ;
#2038 = ORIENTED_EDGE ( 'NONE', *, *, #175, .F. ) ;
#2039 = AXIS2_PLACEMENT_3D ( 'NONE', #2672, #4489, #6704 ) ;
#2040 = DIRECTION ( 'NONE',  ( -5.715354789845005112E-18, -9.999836672264339449E-16, 1.000000000000000000 ) ) ;
#2041 = DIRECTION ( 'NONE',  ( 0.9721221936972340716, 0.2344748185227520376, 0.000000000000000000 ) ) ;
#2042 = CARTESIAN_POINT ( 'NONE',  ( 5.178445921634760474, -62.11857673748845343, 0.8408583081513953950 ) ) ;
#2043 = LINE ( 'NONE', #4352, #1720 ) ;
#2044 = CARTESIAN_POINT ( 'NONE',  ( 3.702507633372579487, -65.47327791553946952, 0.7785861613390434588 ) ) ;
#2045 = VECTOR ( 'NONE', #5813, 1000.000000000000114 ) ;
#2046 = ORIENTED_EDGE ( 'NONE', *, *, #2737, .T. ) ;
#2047 = ORIENTED_EDGE ( 'NONE', *, *, #1363, .F. ) ;
#2048 = ORIENTED_EDGE ( 'NONE', *, *, #3336, .T. ) ;
#2049 = FACE_OUTER_BOUND ( 'NONE', #2128, .T. ) ;
#2050 = CARTESIAN_POINT ( 'NONE',  ( 0.000000000000000000, 0.000000000000000000, -3.000000000000000000 ) ) ;
#2051 = PLANE ( 'NONE',  #4012 ) ;
#2052 = CARTESIAN_POINT ( 'NONE',  ( -3.508682979600159957, -66.46637211483655960, 1.044995729122755179 ) ) ;
#2053 = VERTEX_POINT ( 'NONE', #4796 ) ;
#2054 = ORIENTED_EDGE ( 'NONE', *, *, #761, .F. ) ;
#2055 = ORIENTED_EDGE ( 'NONE', *, *, #3915, .T. ) ;
#2056 = CLOSED_SHELL ( 'NONE', ( #3875, #1473, #2272, #2415, #5080, #1446, #2405, #3622, #6888, #4161, #3472, #5975, #5307, #5806, #5091, #374, #3746, #493, #1624, #3668, #4673, #879, #5647, #6337, #3440, #469, #5984, #2139, #903, #4392, #3140, #6553 ) ) ;
#2057 = DIRECTION ( 'NONE',  ( -0.9999836672264333925, 0.005715354789844970425, 0.000000000000000000 ) ) ;
#2058 = CARTESIAN_POINT ( 'NONE',  ( 3.331090576803830139, -65.95739139720836874, 0.8111086825117052035 ) ) ;
#2059 = CIRCLE ( 'NONE', #520, 1.000000000000001110 ) ;
#2060 = CIRCLE ( 'NONE', #5815, 140.0000000000000000 ) ;
#2061 = CARTESIAN_POINT ( 'NONE',  ( -15.80406914246985650, -35.66025656862317561, -3.575000000000001175E-14 ) ) ;
#2062 = CARTESIAN_POINT ( 'NONE',  ( 18.47982041150265431, -39.47532202006953383, -3.946495907847236140E-14 ) ) ;
#2063 = AXIS2_PLACEMENT_3D ( 'NONE', #4742, #103, #4639 ) ;
#2064 = VERTEX_POINT ( 'NONE', #718 ) ;
#2065 = CIRCLE ( 'NONE', #2676, 2.499999999999997335 ) ;
#2066 = VECTOR ( 'NONE', #1606, 1000.000000000000000 ) ;
#2067 = AXIS2_PLACEMENT_3D ( 'NONE', #3794, #2629, #6116 ) ;
#2068 = CARTESIAN_POINT ( 'NONE',  ( 41.70778007397900211, -94.98992620957551480, 3.999999999999905409 ) ) ;
#2069 = CARTESIAN_POINT ( 'NONE',  ( -14.02739156872318027, -37.17434273187110705, -0.4662714048949997969 ) ) ;
#2070 = PLANE ( 'NONE',  #2073 ) ;
#2071 = EDGE_CURVE ( 'NONE', #3496, #6686, #163, .T. ) ;
#2072 = UNCERTAINTY_MEASURE_WITH_UNIT (LENGTH_MEASURE( 1.000000000000000082E-05 ), #5276, 'distance_accuracy_value', 'NONE');
#2073 = AXIS2_PLACEMENT_3D ( 'NONE', #428, #7230, #6090 ) ;
#2074 = CARTESIAN_POINT ( 'NONE',  ( -14.97059744062764075, -34.32647288175419931, -2.566271404895000163 ) ) ;
#2075 = LINE ( 'NONE', #6125, #5574 ) ;
#2076 = CARTESIAN_POINT ( 'NONE',  ( -3.869447490927095057, -66.24422018797883993, 3.165055290057749993 ) ) ;
#2077 = CARTESIAN_POINT ( 'NONE',  ( -44.78727511552453677, -94.39397278840091587, -3.000000000000095479 ) ) ;
#2078 = CIRCLE ( 'NONE', #6187, 2.249999999999996891 ) ;
#2079 = ORIENTED_EDGE ( 'NONE', *, *, #5189, .F. ) ;
#2080 = LINE ( 'NONE', #6129, #6508 ) ;
#2081 = AXIS2_PLACEMENT_3D ( 'NONE', #6817, #3998, #3955 ) ;
#2082 = DIRECTION ( 'NONE',  ( -0.9979653668924884924, 0.06375834441969779887, 5.805357692931203648E-17 ) ) ;
#2083 = VECTOR ( 'NONE', #433, 1000.000000000000000 ) ;
#2084 = VECTOR ( 'NONE', #3167, 1000.000000000000114 ) ;
#2085 = DIRECTION ( 'NONE',  ( 0.9492883822130744331, -0.3144066910790611624, 0.000000000000000000 ) ) ;
#2086 = ADVANCED_FACE ( 'NONE', ( #3800 ), #7117, .T. ) ;
#2087 = ADVANCED_FACE ( 'NONE', ( #911 ), #824, .F. ) ;
#2088 = CARTESIAN_POINT ( 'NONE',  ( 4.115360779042029904, -63.19255852436059229, -2.695130055691413506 ) ) ;
#2089 = FACE_OUTER_BOUND ( 'NONE', #7077, .T. ) ;
#2090 = CARTESIAN_POINT ( 'NONE',  ( 6.241005725948084226, -61.34940613753865080, 2.614218604193566886 ) ) ;
#2091 = ORIENTED_EDGE ( 'NONE', *, *, #5846, .F. ) ;
#2092 = CIRCLE ( 'NONE', #3656, 11.50000000000000178 ) ;
#2093 = ORIENTED_EDGE ( 'NONE', *, *, #440, .T. ) ;
#2094 = ORIENTED_EDGE ( 'NONE', *, *, #786, .T. ) ;
#2095 = DIRECTION ( 'NONE',  ( 1.000000000000000000, 0.000000000000000000, 0.000000000000000000 ) ) ;
#2096 = CARTESIAN_POINT ( 'NONE',  ( 18.49916120972752154, -39.46430250869199341, 3.499999999999960476 ) ) ;
#2097 = ADVANCED_FACE ( 'NONE', ( #1401 ), #6669, .T. ) ;
#2098 = LINE ( 'NONE', #6656, #3896 ) ;
#2099 = CARTESIAN_POINT ( 'NONE',  ( -5.640317424943829927, -64.23513207997909547, 3.298613272382739936 ) ) ;
#2100 = EDGE_LOOP ( 'NONE', ( #446, #5456, #4019, #5209 ) ) ;
#2101 = FACE_OUTER_BOUND ( 'NONE', #3698, .T. ) ;
#2102 = CARTESIAN_POINT ( 'NONE',  ( 1.919155946380425082, -66.03927477571377835, -1.101811511879709826 ) ) ;
#2103 = CARTESIAN_POINT ( 'NONE',  ( 37.98783301546301061, 6.414454976836671207, -1.055128867088878541 ) ) ;
#2104 = FACE_OUTER_BOUND ( 'NONE', #3497, .T. ) ;
#2105 = ORIENTED_EDGE ( 'NONE', *, *, #4355, .T. ) ;
#2106 = CARTESIAN_POINT ( 'NONE',  ( 11.37011796090756555, -1.723489934710178861, 2.999999999999998224 ) ) ;
#2107 = DIRECTION ( 'NONE',  ( -0.8688689365825387201, -0.4950421911735688463, -4.999999999999992500E-16 ) ) ;
#2108 = DIRECTION ( 'NONE',  ( -5.715354789845005112E-18, -9.999836672264339449E-16, 1.000000000000000000 ) ) ;
#2109 = CARTESIAN_POINT ( 'NONE',  ( -7.117253929586840222, -62.23044735776716152, 0.7381361199122749017 ) ) ;
#2110 = DIRECTION ( 'NONE',  ( -5.715354789860003484E-18, -9.999836672264337477E-16, 1.000000000000000000 ) ) ;
#2111 = ORIENTED_EDGE ( 'NONE', *, *, #4473, .F. ) ;
#2112 = CARTESIAN_POINT ( 'NONE',  ( 15.39542127499540136, -35.83857563806657964, -3.556183125752454544E-14 ) ) ;
#2113 = EDGE_CURVE ( 'NONE', #5269, #4768, #3138, .T. ) ;
#2114 = CARTESIAN_POINT ( 'NONE',  ( 3.888488774788935842, 0.9378992740910084835, -3.000000000000000000 ) ) ;
#2115 = CARTESIAN_POINT ( 'NONE',  ( 41.70778007397900211, -94.98992620957551480, 2.999999999999905409 ) ) ;
#2116 = CARTESIAN_POINT ( 'NONE',  ( -4.410792138572509735, -62.95272468751611683, 0.08690264739508006542 ) ) ;
#2117 = DIRECTION ( 'NONE',  ( -5.715354789845005112E-18, -9.999836672264339449E-16, 1.000000000000000000 ) ) ;
#2118 = CARTESIAN_POINT ( 'NONE',  ( 5.616564958267002083, -63.30981001137231345, -1.476279958498600609 ) ) ;
#2119 = ORIENTED_EDGE ( 'NONE', *, *, #6156, .T. ) ;
#2120 = EDGE_LOOP ( 'NONE', ( #2911, #3182, #6144, #1929 ) ) ;
#2121 = ORIENTED_EDGE ( 'NONE', *, *, #5795, .F. ) ;
#2122 = CARTESIAN_POINT ( 'NONE',  ( 0.000000000000000000, 0.000000000000000000, 0.000000000000000000 ) ) ;
#2123 = DIRECTION ( 'NONE',  ( 1.387778780781445676E-14, 2.775557561562891351E-14, 1.000000000000000000 ) ) ;
#2124 = FACE_OUTER_BOUND ( 'NONE', #2862, .T. ) ;
#2125 = CARTESIAN_POINT ( 'NONE',  ( -12.75609440306747189, -34.09959597428994726, -3.000000000000035083 ) ) ;
#2126 = CARTESIAN_POINT ( 'NONE',  ( 7.168555767344659380, -58.87994835687880624, 1.798531003845740051 ) ) ;
#2127 = ORIENTED_EDGE ( 'NONE', *, *, #310, .T. ) ;
#2128 = EDGE_LOOP ( 'NONE', ( #6898, #105, #4222, #7186 ) ) ;
#2129 = ADVANCED_FACE ( 'NONE', ( #1514 ), #4417, .F. ) ;
#2130 = LINE ( 'NONE', #1617, #7109 ) ;
#2131 = EDGE_CURVE ( 'NONE', #1089, #5892, #6051, .T. ) ;
#2132 = CARTESIAN_POINT ( 'NONE',  ( -14.07431766324680034, -37.03265636863024923, 1.026284428608169819 ) ) ;
#2133 = CARTESIAN_POINT ( 'NONE',  ( -1.892846266465454841, -54.28526762408564110, -0.1610563749503846620 ) ) ;
#2134 = DIRECTION ( 'NONE',  ( -0.9999836672264332815, 0.005715354789859956701, 0.000000000000000000 ) ) ;
#2135 = DIRECTION ( 'NONE',  ( -5.715354789860003484E-18, -9.999836672264337477E-16, 1.000000000000000000 ) ) ;
#2136 = SHAPE_REPRESENTATION ( 'Pivot Pin Rivet', ( #751 ), #1245 ) ;
#2137 = ORIENTED_EDGE ( 'NONE', *, *, #5252, .F. ) ;
#2138 = ORIENTED_EDGE ( 'NONE', *, *, #1602, .F. ) ;
#2139 = ADVANCED_FACE ( 'NONE', ( #6625 ), #3742, .T. ) ;
#2140 = CARTESIAN_POINT ( 'NONE',  ( -20.47590477366745887, -41.48231850745216320, -3.001000000000042522 ) ) ;
#2141 = CARTESIAN_POINT ( 'NONE',  ( 14.49911764349215915, -35.75048010860329839, 2.597518595105000383 ) ) ;
#2142 = CARTESIAN_POINT ( 'NONE',  ( -6.026503769217380402, -56.70691413961192495, -0.01483612153302480557 ) ) ;
#2143 = LINE ( 'NONE', #3280, #1960 ) ;
#2144 = VECTOR ( 'NONE', #5924, 1000.000000000000227 ) ;
#2145 = ORIENTED_EDGE ( 'NONE', *, *, #1260, .F. ) ;
#2146 = FACE_OUTER_BOUND ( 'NONE', #6290, .T. ) ;
#2147 = CARTESIAN_POINT ( 'NONE',  ( 1.475197934039484071, -55.33068667649028782, 1.900472455802885818 ) ) ;
#2148 = FACE_OUTER_BOUND ( 'NONE', #4292, .T. ) ;
#2149 = ADVANCED_BREP_SHAPE_REPRESENTATION ( '', ( #7175, #751 ), #3032 ) ;
#2150 = APPLICATION_CONTEXT ( 'automotive_design' ) ;
#2151 = LINE ( 'NONE', #6099, #5825 ) ;
#2152 = CARTESIAN_POINT ( 'NONE',  ( -1.241878142352246028, -55.26848170174031338, 1.724521099399885182 ) ) ;
#2153 = CARTESIAN_POINT ( 'NONE',  ( 14.63724902514211834, -35.33341991383040437, 3.658178766884810251 ) ) ;
#2154 = LINE ( 'NONE', #7430, #7216 ) ;
#2155 = ORIENTED_EDGE ( 'NONE', *, *, #4864, .F. ) ;
#2156 = CARTESIAN_POINT ( 'NONE',  ( -3.096824821213254975, -64.92072129780139278, 1.460348123614904514 ) ) ;
#2157 = ORIENTED_EDGE ( 'NONE', *, *, #4559, .F. ) ;
#2158 = ORIENTED_EDGE ( 'NONE', *, *, #15, .T. ) ;
#2159 = EDGE_LOOP ( 'NONE', ( #4458, #6760, #2983, #5912 ) ) ;
#2160 = CARTESIAN_POINT ( 'NONE',  ( -18.11931019897951955, 14.08535735325398619, -2.729487737349305831 ) ) ;
#2161 = ORIENTED_EDGE ( 'NONE', *, *, #206, .F. ) ;
#2162 = DIRECTION ( 'NONE',  ( 0.9492883822130744331, -0.3144066910790611624, 0.000000000000000000 ) ) ;
#2163 = CYLINDRICAL_SURFACE ( 'NONE', #3535, 2.250000000000031974 ) ;
#2164 = AXIS2_PLACEMENT_3D ( 'NONE', #6487, #2981, #1757 ) ;
#2165 = DIRECTION ( 'NONE',  ( -5.715354789845005112E-18, -9.999836672264339449E-16, 1.000000000000000000 ) ) ;
#2166 = CARTESIAN_POINT ( 'NONE',  ( -1.678659834933539985, -53.30027862203323252, 1.268182062803870247 ) ) ;
#2167 = EDGE_CURVE ( 'NONE', #3782, #1414, #1430, .T. ) ;
#2168 = DIRECTION ( 'NONE',  ( 0.2223157560262044585, -0.6712493609847989262, 0.7071067811865449082 ) ) ;
#2169 = LINE ( 'NONE', #5623, #3026 ) ;
#2170 = CARTESIAN_POINT ( 'NONE',  ( 5.619938529503549773, -63.59344562873818774, 0.6343307546824898946 ) ) ;
#2171 = LINE ( 'NONE', #3951, #5298 ) ;
#2172 = EDGE_CURVE ( 'NONE', #5715, #1377, #2786, .T. ) ;
#2173 = DIRECTION ( 'NONE',  ( -5.715354789860003484E-18, -9.999836672264337477E-16, 1.000000000000000000 ) ) ;
#2174 = CIRCLE ( 'NONE', #6399, 20.00000000000000000 ) ;
#2175 = ORIENTED_EDGE ( 'NONE', *, *, #6428, .F. ) ;
#2176 = AXIS2_PLACEMENT_3D ( 'NONE', #615, #2903, #5638 ) ;
#2177 = AXIS2_PLACEMENT_3D ( 'NONE', #6222, #1055, #530 ) ;
#2178 = DIRECTION ( 'NONE',  ( -5.715354789860003484E-18, -9.999836672264337477E-16, 1.000000000000000000 ) ) ;
#2179 = DIRECTION ( 'NONE',  ( 0.4364886600403651840, -0.1927644473149899840, -0.8788171126619650497 ) ) ;
#2180 = EDGE_CURVE ( 'NONE', #364, #7163, #3274, .T. ) ;
#2181 = DIRECTION ( 'NONE',  ( -1.602374898470634869E-16, 1.442524254523139935E-17, 1.000000000000000000 ) ) ;
#2182 = CARTESIAN_POINT ( 'NONE',  ( -3.760984799052800476, -54.43314106586858969, -1.957528877657078059 ) ) ;
#2183 = FACE_OUTER_BOUND ( 'NONE', #250, .T. ) ;
#2184 = CIRCLE ( 'NONE', #5086, 2.249999999999962252 ) ;
#2185 = CIRCLE ( 'NONE', #7358, 1.000000000000001776 ) ;
#2186 = VERTEX_POINT ( 'NONE', #3764 ) ;
#2187 = CIRCLE ( 'NONE', #4239, 147.0000000000000000 ) ;
#2188 = CARTESIAN_POINT ( 'NONE',  ( -13.76286933773225130, 13.32929763200878881, -0.3999035282155013471 ) ) ;
#2189 = CARTESIAN_POINT ( 'NONE',  ( -4.871804169514039273, -62.10086352108921659, 3.270302337133240478 ) ) ;
#2190 = CARTESIAN_POINT ( 'NONE',  ( 25.15036705625666258, 26.15624279088187265, 2.645453300864630819E-14 ) ) ;
#2191 = AXIS2_PLACEMENT_3D ( 'NONE', #5067, #2005, #1710 ) ;
#2192 = AXIS2_PLACEMENT_3D ( 'NONE', #5539, #6611, #4470 ) ;
#2193 = LINE ( 'NONE', #2867, #1950 ) ;
#2194 = ADVANCED_FACE ( 'NONE', ( #3198 ), #4514, .T. ) ;
#2195 = CARTESIAN_POINT ( 'NONE',  ( 4.334569312604970470, -57.80406557947362245, -0.9730881136235148832 ) ) ;
#2196 = AXIS2_PLACEMENT_3D ( 'NONE', #2934, #679, #1176 ) ;
#2197 = DIRECTION ( 'NONE',  ( 0.3128416502900965290, -0.9445788350777319931, 0.09950339776592478924 ) ) ;
#2198 = LINE ( 'NONE', #475, #7 ) ;
#2199 = ORIENTED_EDGE ( 'NONE', *, *, #5966, .T. ) ;
#2200 = CARTESIAN_POINT ( 'NONE',  ( 3.594547628745600409, -65.86039197651267330, -3.372550074330296965 ) ) ;
#2201 = ORIENTED_EDGE ( 'NONE', *, *, #1439, .T. ) ;
#2202 = AXIS2_PLACEMENT_3D ( 'NONE', #5057, #1028, #5708 ) ;
#2203 = EDGE_LOOP ( 'NONE', ( #1705, #5259, #2016, #2577 ) ) ;
#2204 = VERTEX_POINT ( 'NONE', #1148 ) ;
#2205 = AXIS2_PLACEMENT_3D ( 'NONE', #1317, #4711, #4898 ) ;
#2206 = ITEM_DEFINED_TRANSFORMATION ( 'NONE', 'NONE', #997,  #751 ) ;
#2207 = LINE ( 'NONE', #4520, #2681 ) ;
#2208 = FACE_OUTER_BOUND ( 'NONE', #4439, .T. ) ;
#2209 = CARTESIAN_POINT ( 'NONE',  ( 0.000000000000000000, 0.000000000000000000, 3.500000000000000000 ) ) ;
#2210 = CARTESIAN_POINT ( 'NONE',  ( -4.011890603535904987, -66.29221981733677183, 1.575336318554399595 ) ) ;
#2211 = ORIENTED_EDGE ( 'NONE', *, *, #5854, .F. ) ;
#2212 = AXIS2_PLACEMENT_3D ( 'NONE', #313, #6561, #6592 ) ;
#2213 = ORIENTED_EDGE ( 'NONE', *, *, #4137, .T. ) ;
#2214 = DIRECTION ( 'NONE',  ( 0.9492899500389723189, 0.3144019573014865121, 0.000000000000000000 ) ) ;
#2215 = EDGE_CURVE ( 'NONE', #6877, #6097, #2260, .T. ) ;
#2216 = CYLINDRICAL_SURFACE ( 'NONE', #6175, 2.500000000000000000 ) ;
#2217 = CARTESIAN_POINT ( 'NONE',  ( -5.895051854024569771, -62.45358532148892294, 3.505907163650189950 ) ) ;
#2218 = AXIS2_PLACEMENT_3D ( 'NONE', #1419, #4818, #3709 ) ;
#2219 = CARTESIAN_POINT ( 'NONE',  ( 35.25551690214635414, 7.283442040853450372, -2.999999999999993339 ) ) ;
#2220 = CARTESIAN_POINT ( 'NONE',  ( -95.86211798318534250, -102.0316339954322018, -1.025655255171287195E-13 ) ) ;
#2221 = CARTESIAN_POINT ( 'NONE',  ( 30.52077159997833533, 5.488396937353885896, -1.499999999999994893 ) ) ;
#2222 = ORIENTED_EDGE ( 'NONE', *, *, #5148, .F. ) ;
#2223 = ORIENTED_EDGE ( 'NONE', *, *, #3784, .F. ) ;
#2224 = ADVANCED_FACE ( 'NONE', ( #7339 ), #6194, .F. ) ;
#2225 = EDGE_CURVE ( 'NONE', #6135, #321, #5322, .T. ) ;
#2226 = CARTESIAN_POINT ( 'NONE',  ( 18.06432739836606771, -39.71205113188410962, 2.999999999999959144 ) ) ;
#2227 = CARTESIAN_POINT ( 'NONE',  ( 39.32685927492619982, -94.35036853610694152, -9.410874857174178487E-14 ) ) ;
#2228 = CARTESIAN_POINT ( 'NONE',  ( 27.55235279947361349, -34.38166451341171381, -3.421263025543810879E-14 ) ) ;
#2229 = CARTESIAN_POINT ( 'NONE',  ( -6.994430249510970476, -62.66069223349322925, -1.382237850844937777 ) ) ;
#2230 = CARTESIAN_POINT ( 'NONE',  ( -28.22553731214382111, -35.79092421365019305, -3.595165860846261460E-14 ) ) ;
#2231 = ORIENTED_EDGE ( 'NONE', *, *, #6450, .F. ) ;
#2232 = CARTESIAN_POINT ( 'NONE',  ( 30.67250997583011696, 4.753907001892617501, -1.499999999999995559 ) ) ;
#2233 = EDGE_CURVE ( 'NONE', #5807, #6679, #6638, .T. ) ;
#2234 = EDGE_CURVE ( 'NONE', #577, #5033, #2824, .T. ) ;
#2235 = CARTESIAN_POINT ( 'NONE',  ( 4.334569312604970470, -57.80406557947362245, -0.9730881136235148832 ) ) ;
#2236 = DIRECTION ( 'NONE',  ( -1.850371707708594129E-14, -4.394632805807911095E-14, 1.000000000000000000 ) ) ;
#2237 = LINE ( 'NONE', #4510, #2564 ) ;
#2238 = CARTESIAN_POINT ( 'NONE',  ( 4.469984187763964556, -63.33186444122004843, 2.519959534738519746 ) ) ;
#2239 = CARTESIAN_POINT ( 'NONE',  ( -19.02987527034469650, -39.22028924617138301, -3.000000000000040412 ) ) ;
#2240 = CARTESIAN_POINT ( 'NONE',  ( 37.86567095459282228, 7.005780695865149177, -1.500000000001998623 ) ) ;
#2241 = ORIENTED_EDGE ( 'NONE', *, *, #6655, .F. ) ;
#2242 = EDGE_LOOP ( 'NONE', ( #282, #1407 ) ) ;
#2243 = VERTEX_POINT ( 'NONE', #5629 ) ;
#2244 = SHAPE_DEFINITION_REPRESENTATION ( #4288, #2136 ) ;
#2245 = DIRECTION ( 'NONE',  ( 0.9147661038495522590, -0.4039838799357101107, 0.000000000000000000 ) ) ;
#2246 = ORIENTED_EDGE ( 'NONE', *, *, #6154, .F. ) ;
#2247 = DIRECTION ( 'NONE',  ( 5.715354789845005112E-18, 9.999836672264339449E-16, -1.000000000000000000 ) ) ;
#2248 = DIRECTION ( 'NONE',  ( 0.9222310071080526139, 0.3866393274467394559, 3.919038899579848814E-16 ) ) ;
#2249 = PLANE ( 'NONE',  #2332 ) ;
#2250 = CARTESIAN_POINT ( 'NONE',  ( 2.327488905229944560, -67.40324771348248589, -1.912586833593244773 ) ) ;
#2251 = ORIENTED_EDGE ( 'NONE', *, *, #7295, .T. ) ;
#2252 = ORIENTED_EDGE ( 'NONE', *, *, #3180, .F. ) ;
#2253 = CARTESIAN_POINT ( 'NONE',  ( -20.83603634162975737, 9.201721367189403367, 0.4060579846639940094 ) ) ;
#2254 = CARTESIAN_POINT ( 'NONE',  ( 18.47982041150265431, -39.47532202006953383, 2.999999999999960476 ) ) ;
#2255 = CARTESIAN_POINT ( 'NONE',  ( 13.49911764349216092, -35.75048010860329839, 0.4975185951050001831 ) ) ;
#2256 = CARTESIAN_POINT ( 'NONE',  ( -15.49899450467540163, -35.75040780681265318, -2.566271404894997499 ) ) ;
#2257 = CARTESIAN_POINT ( 'NONE',  ( 0.000000000000000000, 0.000000000000000000, 0.000000000000000000 ) ) ;
#2258 = LINE ( 'NONE', #4605, #6391 ) ;
#2259 = ORIENTED_EDGE ( 'NONE', *, *, #3785, .T. ) ;
#2260 = LINE ( 'NONE', #1745, #5571 ) ;
#2261 = DIRECTION ( 'NONE',  ( -0.1676281164441980331, -0.9858503002877112564, -9.867922527762208252E-16 ) ) ;
#2262 = DIRECTION ( 'NONE',  ( -0.9721221936972339606, -0.2344748185227521209, -0.000000000000000000 ) ) ;
#2263 = CARTESIAN_POINT ( 'NONE',  ( -1.564844514157090138, -53.52797147715784121, 0.2502733031487548443 ) ) ;
#2264 = EDGE_CURVE ( 'NONE', #2912, #6662, #269, .T. ) ;
#2265 = LINE ( 'NONE', #1552, #5593 ) ;
#2266 = ORIENTED_EDGE ( 'NONE', *, *, #4302, .F. ) ;
#2267 = CARTESIAN_POINT ( 'NONE',  ( -4.747355111503322789, -62.01643032957871071, 2.629496613306467445 ) ) ;
#2268 = CARTESIAN_POINT ( 'NONE',  ( 18.74668230531428748, -39.89873697698326538, -1.000000000000039968 ) ) ;
#2269 = DIRECTION ( 'NONE',  ( -0.2163384215910431896, -0.07165063022625259292, 0.9736857165079894072 ) ) ;
#2270 = CARTESIAN_POINT ( 'NONE',  ( -4.423017985506799477, -63.40237279495851652, -1.015450938335749953 ) ) ;
#2271 = CARTESIAN_POINT ( 'NONE',  ( -28.37794841333321116, 12.47776197281416088, -1.499999999999988010 ) ) ;
#2272 = ADVANCED_FACE ( 'NONE', ( #3351 ), #5663, .T. ) ;
#2273 = CARTESIAN_POINT ( 'NONE',  ( 3.705224094368697152, -65.54171936622607575, -1.318943324162216824 ) ) ;
#2274 = ADVANCED_FACE ( 'NONE', ( #605 ), #1588, .F. ) ;
#2275 = ORIENTED_EDGE ( 'NONE', *, *, #4644, .F. ) ;
#2276 = VERTEX_POINT ( 'NONE', #3390 ) ;
#2277 = ORIENTED_EDGE ( 'NONE', *, *, #6598, .F. ) ;
#2278 = CIRCLE ( 'NONE', #6485, 5.000000000000000000 ) ;
#2279 = FACE_OUTER_BOUND ( 'NONE', #158, .T. ) ;
#2280 = VERTEX_POINT ( 'NONE', #540 ) ;
#2281 = DIRECTION ( 'NONE',  ( -5.715354789845005112E-18, -9.999836672264339449E-16, 1.000000000000000000 ) ) ;
#2282 = CARTESIAN_POINT ( 'NONE',  ( -15.08175531864075047, -33.99084820126180517, -5.041145139047909396 ) ) ;
#2283 = CARTESIAN_POINT ( 'NONE',  ( 27.23210503485723777, -35.06560599256804522, -1.000000000000034861 ) ) ;
#2284 = CARTESIAN_POINT ( 'NONE',  ( 1.647105754412080181, -53.29316706828264216, -0.6741030570719998005 ) ) ;
#2285 = ORIENTED_EDGE ( 'NONE', *, *, #3915, .F. ) ;
#2286 = CIRCLE ( 'NONE', #243, 0.9999999999999998890 ) ;
#2287 = ORIENTED_EDGE ( 'NONE', *, *, #4540, .T. ) ;
#2288 = CARTESIAN_POINT ( 'NONE',  ( -14.70408710852078116, -35.66654345889202204, -3.000000000000036415 ) ) ;
#2289 = DIRECTION ( 'NONE',  ( -5.715354789845005112E-18, -9.999836672264339449E-16, 1.000000000000000000 ) ) ;
#2290 = LINE ( 'NONE', #6334, #4749 ) ;
#2291 = CARTESIAN_POINT ( 'NONE',  ( -16.40387102536037744, 1.778486824056639826, 1.734723475976807094E-15 ) ) ;
#2292 = CARTESIAN_POINT ( 'NONE',  ( 37.74350889372263396, 7.597106414893625370, -1.944871132915118705 ) ) ;
#2293 = LINE ( 'NONE', #4103, #4216 ) ;
#2294 = ORIENTED_EDGE ( 'NONE', *, *, #3052, .F. ) ;
#2295 = DIRECTION ( 'NONE',  ( -5.715354789845005112E-18, -9.999836672264339449E-16, 1.000000000000000000 ) ) ;
#2296 = CARTESIAN_POINT ( 'NONE',  ( -5.071543166975963857, -62.10633079430171222, 1.661898009719716462 ) ) ;
#2297 = CARTESIAN_POINT ( 'NONE',  ( 0.4505070138924615053, -66.21322040523499197, 1.114523354903560248 ) ) ;
#2298 = CARTESIAN_POINT ( 'NONE',  ( -2.273841640848679901, -67.16083533941571204, 1.488471302465715018 ) ) ;
#2299 = FACE_OUTER_BOUND ( 'NONE', #211, .T. ) ;
#2300 = EDGE_LOOP ( 'NONE', ( #5053, #3127, #2094, #1284 ) ) ;
#2301 = VECTOR ( 'NONE', #1556, 1000.000000000000114 ) ;
#2302 = CARTESIAN_POINT ( 'NONE',  ( 18.52216156081266618, -40.03310245541522505, 3.974029017541355291 ) ) ;
#2303 = AXIS2_PLACEMENT_3D ( 'NONE', #1883, #6590, #1429 ) ;
#2304 = CARTESIAN_POINT ( 'NONE',  ( 39.48483786921892857, -95.33781693134928048, 2.999999999999904521 ) ) ;
#2305 = EDGE_CURVE ( 'NONE', #7415, #4629, #5140, .T. ) ;
#2306 = DIRECTION ( 'NONE',  ( 0.3128463504745285229, 0.9445772445362839997, 0.09950371902099811039 ) ) ;
#2307 = DIRECTION ( 'NONE',  ( 0.1546180985661289864, -0.9879743132267128081, -9.870744795757291736E-16 ) ) ;
#2308 = AXIS2_PLACEMENT_3D ( 'NONE', #193, #1258, #86 ) ;
#2309 = CARTESIAN_POINT ( 'NONE',  ( 5.768687865266859838, -59.13854474313614418, 2.609246528188839509 ) ) ;
#2310 = AXIS2_PLACEMENT_3D ( 'NONE', #924, #3737, #6684 ) ;
#2311 = DIRECTION ( 'NONE',  ( -0.8545275983175482093, -0.5194059912184716410, -5.242814362801270410E-16 ) ) ;
#2312 = CARTESIAN_POINT ( 'NONE',  ( -33.94153943842304955, 12.25650441806195801, -2.999999999999988898 ) ) ;
#2313 = ORIENTED_EDGE ( 'NONE', *, *, #1682, .T. ) ;
#2314 = B_SPLINE_CURVE_WITH_KNOTS ( 'NONE', 3,
 ( #1543, #5624, #457, #376 ),
 .UNSPECIFIED., .F., .F.,
 ( 4, 4 ),
 ( 0.000000000000000000, 1.000000000000000000 ),
 .UNSPECIFIED. ) ;
#2315 = AXIS2_PLACEMENT_3D ( 'NONE', #59, #1752, #7105 ) ;
#2316 = EDGE_LOOP ( 'NONE', ( #5009, #2813, #6458 ) ) ;
#2317 = VERTEX_POINT ( 'NONE', #1218 ) ;
#2318 = VERTEX_POINT ( 'NONE', #3046 ) ;
#2319 = VECTOR ( 'NONE', #5639, 1000.000000000000000 ) ;
#2320 = AXIS2_PLACEMENT_3D ( 'NONE', #1453, #4896, #4404 ) ;
#2321 = CONTEXT_DEPENDENT_SHAPE_REPRESENTATION ( #1498, #2955 ) ;
#2322 = EDGE_CURVE ( 'NONE', #4812, #489, #32, .T. ) ;
#2323 = FACE_OUTER_BOUND ( 'NONE', #3428, .T. ) ;
#2324 = CARTESIAN_POINT ( 'NONE',  ( 24.99346688245966419, 26.01411140189437532, -2.993845543551503674 ) ) ;
#2325 = CARTESIAN_POINT ( 'NONE',  ( 6.493768279116130415, -62.63809584774485018, -3.239169643854469705 ) ) ;
#2326 = CARTESIAN_POINT ( 'NONE',  ( 27.29329919813223526, -34.45380074488651445, -0.1316498810018032206 ) ) ;
#2327 = CARTESIAN_POINT ( 'NONE',  ( -1.435618805647706164, -65.69410370267330279, -0.7494494782121799981 ) ) ;
#2328 = VERTEX_POINT ( 'NONE', #1879 ) ;
#2329 = AXIS2_PLACEMENT_3D ( 'NONE', #6671, #314, #1432 ) ;
#2330 = AXIS2_PLACEMENT_3D ( 'NONE', #244, #3064, #6492 ) ;
#2331 = ORIENTED_EDGE ( 'NONE', *, *, #4170, .F. ) ;
#2332 = AXIS2_PLACEMENT_3D ( 'NONE', #5040, #3221, #1535 ) ;
#2333 = DIRECTION ( 'NONE',  ( -0.8474369140690223290, 0.5308961072311347840, 5.260440335992994916E-16 ) ) ;
#2334 = EDGE_CURVE ( 'NONE', #6921, #210, #4235, .T. ) ;
#2335 = DIRECTION ( 'NONE',  ( 0.000000000000000000, 0.000000000000000000, 1.000000000000000000 ) ) ;
#2336 = FACE_OUTER_BOUND ( 'NONE', #1233, .T. ) ;
#2337 = AXIS2_PLACEMENT_3D ( 'NONE', #1431, #3616, #825 ) ;
#2338 = AXIS2_PLACEMENT_3D ( 'NONE', #6911, #1943, #2902 ) ;
#2339 = CYLINDRICAL_SURFACE ( 'NONE', #5950, 5.000000000000000000 ) ;
#2340 = DIRECTION ( 'NONE',  ( 0.9999836672264332815, -0.005715354789845002517, 0.000000000000000000 ) ) ;
#2341 = CARTESIAN_POINT ( 'NONE',  ( 12.15447797363371052, 11.01039466689934443, 1.127570259384924611E-14 ) ) ;
#2342 = VERTEX_POINT ( 'NONE', #651 ) ;
#2343 = ORIENTED_EDGE ( 'NONE', *, *, #4303, .F. ) ;
#2344 = AXIS2_PLACEMENT_3D ( 'NONE', #187, #5308, #641 ) ;
#2345 = ADVANCED_FACE ( 'NONE', ( #5923 ), #2485, .T. ) ;
#2346 =( LENGTH_UNIT ( ) NAMED_UNIT ( * ) SI_UNIT ( .MILLI., .METRE. ) );
#2347 = PLANE ( 'NONE',  #2081 ) ;
#2348 = CARTESIAN_POINT ( 'NONE',  ( 14.63724902514211834, -35.33341991383040437, 3.658178766884810251 ) ) ;
#2349 = CARTESIAN_POINT ( 'NONE',  ( -7.922926035662746003, 12.41525034409755612, 2.701156757981117984 ) ) ;
#2350 = ORIENTED_EDGE ( 'NONE', *, *, #6966, .F. ) ;
#2351 = CARTESIAN_POINT ( 'NONE',  ( -4.748090069711009775, -62.01667038360579198, 2.533819555318849837 ) ) ;
#2352 = CARTESIAN_POINT ( 'NONE',  ( 7.529070345495034289, 16.11642554373085900, 3.000000000000015987 ) ) ;
#2353 = CARTESIAN_POINT ( 'NONE',  ( -19.02987527034469650, -39.22028924617138301, -3.932841115884471972E-14 ) ) ;
#2354 = CARTESIAN_POINT ( 'NONE',  ( 2.799893819535080208, -55.23287331081275653, 0.2233987335540700003 ) ) ;
#2355 = CARTESIAN_POINT ( 'NONE',  ( -1.512046953658800152, -54.18079592905042574, 1.959428465566195543 ) ) ;
#2356 = DIRECTION ( 'NONE',  ( 0.3128463504745289669, 0.9445772445362837777, 0.09950371902099887367 ) ) ;
#2357 = ADVANCED_FACE ( 'NONE', ( #3499 ), #6967, .T. ) ;
#2358 = ORIENTED_EDGE ( 'NONE', *, *, #5283, .T. ) ;
#2359 = ORIENTED_EDGE ( 'NONE', *, *, #5447, .F. ) ;
#2360 = PLANE ( 'NONE',  #7252 ) ;
#2361 = CARTESIAN_POINT ( 'NONE',  ( 15.82006518139326978, 14.33094549030128029, -2.230393353321955541 ) ) ;
#2362 = CARTESIAN_POINT ( 'NONE',  ( -5.316774007586650086, -63.89131393482077925, 1.354123676545745170 ) ) ;
#2363 = CARTESIAN_POINT ( 'NONE',  ( 27.96836146114586441, -34.65561064741672226, -0.2632997616376124284 ) ) ;
#2364 = ORIENTED_EDGE ( 'NONE', *, *, #1900, .T. ) ;
#2365 = EDGE_CURVE ( 'NONE', #5988, #4812, #2059, .T. ) ;
#2366 = ORIENTED_EDGE ( 'NONE', *, *, #3653, .T. ) ;
#2367 = DIRECTION ( 'NONE',  ( -0.4039838799357098331, -0.9147661038495523700, -8.673617379884154787E-16 ) ) ;
#2368 = CARTESIAN_POINT ( 'NONE',  ( 14.49911764349215915, -35.75048010860329839, 0.4975185951050001831 ) ) ;
#2369 = DIRECTION ( 'NONE',  ( 0.9999836672264332815, -0.005715354789845002517, 0.000000000000000000 ) ) ;
#2370 = CARTESIAN_POINT ( 'NONE',  ( -4.748090069711009775, -62.01667038360579198, 2.533819555318849837 ) ) ;
#2371 = CARTESIAN_POINT ( 'NONE',  ( -6.199032880790720235, -61.56120177486793210, 3.556545127952429830 ) ) ;
#2372 = CARTESIAN_POINT ( 'NONE',  ( 44.95353084483765826, -94.82378791335750634, 3.999999999999905409 ) ) ;
#2373 = ORIENTED_EDGE ( 'NONE', *, *, #621, .T. ) ;
#2374 = EDGE_CURVE ( 'NONE', #5998, #1992, #2669, .T. ) ;
#2375 = ADVANCED_FACE ( 'NONE', ( #4789 ), #3006, .T. ) ;
#2376 = CARTESIAN_POINT ( 'NONE',  ( 1.576955190785845007, -65.26733347271304808, -2.474060432887700500 ) ) ;
#2377 =( NAMED_UNIT ( * ) SI_UNIT ( $, .STERADIAN. ) SOLID_ANGLE_UNIT ( ) );
#2378 = DIRECTION ( 'NONE',  ( 5.715354789845005112E-18, 9.999836672264339449E-16, -1.000000000000000000 ) ) ;
#2379 = FACE_OUTER_BOUND ( 'NONE', #1982, .T. ) ;
#2380 = ORIENTED_EDGE ( 'NONE', *, *, #7023, .F. ) ;
#2381 = DIRECTION ( 'NONE',  ( 0.9999836672264332815, -0.005715354789845002517, 0.000000000000000000 ) ) ;
#2382 = CARTESIAN_POINT ( 'NONE',  ( 18.05682957847944436, -39.71632305027067389, -0.8833408112552532110 ) ) ;
#2383 = CARTESIAN_POINT ( 'NONE',  ( 4.841738599488129680, -63.57854475872899513, -1.322671891113719855 ) ) ;
#2384 = CARTESIAN_POINT ( 'NONE',  ( -5.714251477591489881, -57.46902543231049521, -0.4259505751857597389 ) ) ;
#2385 = DIRECTION ( 'NONE',  ( -0.4328040977884316520, 0.5819352847797604200, 0.6884997728872834788 ) ) ;
#2386 =( BOUNDED_SURFACE ( )  B_SPLINE_SURFACE ( 3, 2, ( 
 ( #2978, #6422, #3055 ),
 ( #1332, #1886, #763 ),
 ( #3661, #5262, #5977 ),
 ( #721, #5935, #1268 ),
 ( #4798, #6482, #4834 ),
 ( #4725, #4160, #3549 ),
 ( #6452, #2382, #3581 ),
 ( #5864, #7081, #3617 ),
 ( #3689, #5896, #5398 ),
 ( #237, #7119, #1958 ) ),
 .UNSPECIFIED., .F., .F., .T. ) 
 B_SPLINE_SURFACE_WITH_KNOTS ( ( 4, 2, 2, 2, 4 ),
 ( 3, 3 ),
 ( 0.000000000000000000, 0.0001953595625521471020, 0.0003907191251042942039, 0.0005860786876564413059, 0.0007814382502085884079 ),
 ( 0.000000000000000000, 1.000000000000000000 ),
 .UNSPECIFIED. ) 
 GEOMETRIC_REPRESENTATION_ITEM ( )  RATIONAL_B_SPLINE_SURFACE ( (
 ( 1.000000000000000000, 0.6917656125192643835, 1.000000000000000000),
 ( 1.000000000000000000, 0.6917626678221141523, 1.000000000000000000),
 ( 1.000000000000000000, 0.6921708295056779869, 1.000000000000000000),
 ( 1.000000000000000000, 0.6937291441607075226, 1.000000000000000000),
 ( 1.000000000000000000, 0.6948807116037144516, 1.000000000000000000),
 ( 1.000000000000000000, 0.6977261400977853301, 1.000000000000000000),
 ( 1.000000000000000000, 0.6994400533938299747, 1.000000000000000000),
 ( 1.000000000000000000, 0.7031153542365370379, 1.000000000000000000),
 ( 1.000000000000000000, 0.7051186676678535825, 1.000000000000000000),
 ( 1.000000000000000000, 0.7071067811865472397, 1.000000000000000000) ) ) 
 REPRESENTATION_ITEM ( '' )  SURFACE ( )  );
#2387 = ORIENTED_EDGE ( 'NONE', *, *, #749, .F. ) ;
#2388 = VERTEX_POINT ( 'NONE', #5888 ) ;
#2389 = EDGE_LOOP ( 'NONE', ( #3062, #6776, #1824, #6331, #3971 ) ) ;
#2390 = PLANE ( 'NONE',  #4114 ) ;
#2391 = CARTESIAN_POINT ( 'NONE',  ( 0.000000000000000000, 0.000000000000000000, 3.000000000000000000 ) ) ;
#2392 = CARTESIAN_POINT ( 'NONE',  ( -5.951685856498870386, -64.29772444222471961, -2.487703520802049262 ) ) ;
#2393 = CARTESIAN_POINT ( 'NONE',  ( 27.57011700825883693, -34.29608248668765214, -0.6201149797898980465 ) ) ;
#2394 = MANIFOLD_SOLID_BREP ( 'Stock-MAS-689-1', #3615 ) ;
#2395 = VERTEX_POINT ( 'NONE', #1292 ) ;
#2396 = AXIS2_PLACEMENT_3D ( 'NONE', #377, #1544, #2671 ) ;
#2397 = DIRECTION ( 'NONE',  ( 0.000000000000000000, 0.000000000000000000, -1.000000000000000000 ) ) ;
#2398 = EDGE_CURVE ( 'NONE', #4056, #5232, #4136, .T. ) ;
#2399 = FACE_OUTER_BOUND ( 'NONE', #4848, .T. ) ;
#2400 = VECTOR ( 'NONE', #1773, 1000.000000000000000 ) ;
#2401 = DIRECTION ( 'NONE',  ( -0.9999836672264333925, 0.005715354789844388425, 0.000000000000000000 ) ) ;
#2402 = FACE_OUTER_BOUND ( 'NONE', #5996, .T. ) ;
#2403 = CARTESIAN_POINT ( 'NONE',  ( 5.360452058498115235, -63.64145676321751921, 2.745338867839514752 ) ) ;
#2404 = VECTOR ( 'NONE', #1098, 1000.000000000000000 ) ;
#2405 = ADVANCED_FACE ( 'NONE', ( #1570 ), #1947, .T. ) ;
#2406 = EDGE_CURVE ( 'NONE', #2620, #6077, #986, .T. ) ;
#2407 = CARTESIAN_POINT ( 'NONE',  ( 0.000000000000000000, 0.000000000000000000, 3.000000000000000000 ) ) ;
#2408 = CARTESIAN_POINT ( 'NONE',  ( 4.106052318423260239, -56.36209498175141874, 0.3538987277600479375 ) ) ;
#2409 = AXIS2_PLACEMENT_3D ( 'NONE', #5567, #3850, #443 ) ;
#2410 = PRODUCT_DEFINITION_SHAPE ( 'NONE', 'NONE',  #5025 ) ;
#2411 = CARTESIAN_POINT ( 'NONE',  ( -6.176129832103540274, -61.75772637036916279, 1.476179264717100370 ) ) ;
#2412 = ORIENTED_EDGE ( 'NONE', *, *, #7033, .T. ) ;
#2413 = CARTESIAN_POINT ( 'NONE',  ( -4.759129193302329419, -62.02058092981934578, 2.720659859784867241 ) ) ;
#2414 = CIRCLE ( 'NONE', #2654, 11.50000000000000178 ) ;
#2415 = ADVANCED_FACE ( 'NONE', ( #4297 ), #1938, .T. ) ;
#2416 = FACE_BOUND ( 'NONE', #6516, .T. ) ;
#2417 = MANIFOLD_SOLID_BREP ( 'NONE', #3133 ) ;
#2418 = CARTESIAN_POINT ( 'NONE',  ( -5.794328821513979655, -59.26142744441108334, -0.3953236866292048068 ) ) ;
#2419 = CARTESIAN_POINT ( 'NONE',  ( 5.416018991692120643, -63.93240027730202968, 2.754852738177090643 ) ) ;
#2420 = CARTESIAN_POINT ( 'NONE',  ( -14.49899450467539985, -35.75040780681265318, -2.566271404894997499 ) ) ;
#2421 = EDGE_LOOP ( 'NONE', ( #4697, #4071, #2541, #3463 ) ) ;
#2422 = ORIENTED_EDGE ( 'NONE', *, *, #4441, .F. ) ;
#2423 = EDGE_LOOP ( 'NONE', ( #3444, #4285, #6104, #5051, #2331 ) ) ;
#2424 = EDGE_LOOP ( 'NONE', ( #6067, #4558 ) ) ;
#2425 = DIRECTION ( 'NONE',  ( 0.3128416502900965290, -0.9445788350777318820, 0.09950339776592408148 ) ) ;
#2426 = CIRCLE ( 'NONE', #3880, 2.999999999999999556 ) ;
#2427 = CIRCLE ( 'NONE', #2780, 5.000000000000000000 ) ;
#2428 = DIRECTION ( 'NONE',  ( 0.4039838799357093335, 0.9147661038495527031, 1.550530988647994607E-16 ) ) ;
#2429 = CARTESIAN_POINT ( 'NONE',  ( 1.647567807763375081, -53.54661630431167652, -1.692287459705078101 ) ) ;
#2430 = CARTESIAN_POINT ( 'NONE',  ( 13.32147353159843028, 12.06754263290683937, -0.3999035282155026794 ) ) ;
#2431 = VERTEX_POINT ( 'NONE', #3682 ) ;
#2432 = AXIS2_PLACEMENT_3D ( 'NONE', #6256, #1802, #566 ) ;
#2433 = AXIS2_PLACEMENT_3D ( 'NONE', #4645, #7410, #531 ) ;
#2434 =( LENGTH_UNIT ( ) NAMED_UNIT ( * ) SI_UNIT ( .MILLI., .METRE. ) );
#2435 = LINE ( 'NONE', #6469, #3401 ) ;
#2436 = CIRCLE ( 'NONE', #7007, 17.99999999999999645 ) ;
#2437 = CARTESIAN_POINT ( 'NONE',  ( 0.000000000000000000, 0.000000000000000000, 3.000000000000000000 ) ) ;
#2438 = CIRCLE ( 'NONE', #277, 2.999999999999999556 ) ;
#2439 = CARTESIAN_POINT ( 'NONE',  ( 104.0973215944787711, -119.5240462704291389, -3.000000000000119904 ) ) ;
#2440 = DIRECTION ( 'NONE',  ( 5.715354789845005112E-18, 9.999836672264339449E-16, -1.000000000000000000 ) ) ;
#2441 = PRODUCT_DEFINITION_FORMATION_WITH_SPECIFIED_SOURCE ( 'ANY', '', #196, .NOT_KNOWN. ) ;
#2442 = VECTOR ( 'NONE', #412, 1000.000000000000000 ) ;
#2443 = ORIENTED_EDGE ( 'NONE', *, *, #6156, .F. ) ;
#2444 = EDGE_CURVE ( 'NONE', #4550, #106, #4844, .T. ) ;
#2445 = AXIS2_PLACEMENT_3D ( 'NONE', #5326, #2529, #1297 ) ;
#2446 = CARTESIAN_POINT ( 'NONE',  ( -2.889418079045375176, -55.97554976774797098, -0.4852521485111498389 ) ) ;
#2447 = AXIS2_PLACEMENT_3D ( 'NONE', #6860, #1783, #1222 ) ;
#2448 = CIRCLE ( 'NONE', #1488, 140.0000000000000000 ) ;
#2449 = DIRECTION ( 'NONE',  ( 0.4039838799357101107, 0.9147661038495522590, 4.900000000000001209E-14 ) ) ;
#2450 = CARTESIAN_POINT ( 'NONE',  ( 5.071800925510882685, -62.16193033951381608, -3.298373296383677822 ) ) ;
#2451 = CARTESIAN_POINT ( 'NONE',  ( -5.712169679815763068, -59.50909061234685993, -0.3802802853964926122 ) ) ;
#2452 = CIRCLE ( 'NONE', #2699, 1.000000000000000444 ) ;
#2453 = ORIENTED_EDGE ( 'NONE', *, *, #5246, .F. ) ;
#2454 = EDGE_CURVE ( 'NONE', #364, #5643, #4826, .T. ) ;
#2455 = EDGE_CURVE ( 'NONE', #1198, #3782, #2184, .T. ) ;
#2456 = CARTESIAN_POINT ( 'NONE',  ( 27.55235279947361349, -34.38166451341158592, 3.999999999999966249 ) ) ;
#2457 = CARTESIAN_POINT ( 'NONE',  ( 18.31184849395284786, -40.14648560017537449, -3.998375596128007773E-14 ) ) ;
#2458 = CARTESIAN_POINT ( 'NONE',  ( -0.9378992740910081505, 3.888488774788935842, 3.000000000000000000 ) ) ;
#2459 = UNCERTAINTY_MEASURE_WITH_UNIT (LENGTH_MEASURE( 1.000000000000000082E-05 ), #1246, 'distance_accuracy_value', 'NONE');
#2460 = DIRECTION ( 'NONE',  ( 0.2223157560262044585, -0.6712493609847989262, 0.7071067811865449082 ) ) ;
#2461 = CARTESIAN_POINT ( 'NONE',  ( 4.980378365057210210, -62.14367890036703557, -3.355420260138584521 ) ) ;
#2462 = CARTESIAN_POINT ( 'NONE',  ( -6.599700898649300207, -61.96243991103532522, 3.420662994399620072 ) ) ;
#2463 = CARTESIAN_POINT ( 'NONE',  ( 3.749938752099124972, -0.02143258046197201241, -3.000000000000000888 ) ) ;
#2464 = EDGE_LOOP ( 'NONE', ( #5179, #6528, #4468, #3270, #3678, #6357 ) ) ;
#2465 = ADVANCED_FACE ( 'NONE', ( #1424 ), #1394, .T. ) ;
#2466 = EDGE_CURVE ( 'NONE', #420, #5434, #6057, .T. ) ;
#2467 = ORIENTED_EDGE ( 'NONE', *, *, #6733, .F. ) ;
#2468 = ORIENTED_EDGE ( 'NONE', *, *, #4815, .F. ) ;
#2469 = DIRECTION ( 'NONE',  ( -0.9721221936972339606, -0.2344748185227520376, 0.000000000000000000 ) ) ;
#2470 = EDGE_LOOP ( 'NONE', ( #5660, #7344, #4658, #3206 ) ) ;
#2471 = PLANE ( 'NONE',  #4372 ) ;
#2472 = CARTESIAN_POINT ( 'NONE',  ( -5.509265921604280081, -56.99747518668161206, -0.3692125993829896702 ) ) ;
#2473 = LINE ( 'NONE', #733, #2084 ) ;
#2474 = VERTEX_POINT ( 'NONE', #263 ) ;
#2475 = EDGE_CURVE ( 'NONE', #6355, #327, #146, .T. ) ;
#2476 = ORIENTED_EDGE ( 'NONE', *, *, #6115, .T. ) ;
#2477 = ORIENTED_EDGE ( 'NONE', *, *, #293, .F. ) ;
#2478 = CARTESIAN_POINT ( 'NONE',  ( -22.27644891976294161, 9.837844043328900057, 3.306154456448478829 ) ) ;
#2479 = CARTESIAN_POINT ( 'NONE',  ( 8.411763394295572738, 16.69999280642484507, 3.000000000000017764 ) ) ;
#2480 = CARTESIAN_POINT ( 'NONE',  ( 35.25551690214635414, 7.283442040853450372, -2.999999999999993339 ) ) ;
#2481 = DIRECTION ( 'NONE',  ( -0.9999836672264332815, 0.005715354789845002517, 0.000000000000000000 ) ) ;
#2482 = DIRECTION ( 'NONE',  ( -5.715354789845005112E-18, -9.999836672264339449E-16, 1.000000000000000000 ) ) ;
#2483 = ORIENTED_EDGE ( 'NONE', *, *, #3799, .T. ) ;
#2484 = CARTESIAN_POINT ( 'NONE',  ( -5.155987128177820900, -61.76400128369626685, 1.194474120832875519 ) ) ;
#2485 = PLANE ( 'NONE',  #3264 ) ;
#2486 = CARTESIAN_POINT ( 'NONE',  ( 24.99346688245966419, 26.01411140189437177, 0.006154456448490951831 ) ) ;
#2487 = CARTESIAN_POINT ( 'NONE',  ( -1.869726328446417840, -65.97170341743343158, -2.950226656714010964 ) ) ;
#2488 = CARTESIAN_POINT ( 'NONE',  ( 5.608858804484560423, -63.72364544018660126, -1.429200976399037870 ) ) ;
#2489 = ORIENTED_EDGE ( 'NONE', *, *, #1994, .T. ) ;
#2490 = DIRECTION ( 'NONE',  ( 0.1860016876085203441, -0.1636620475539279917, 0.9688230521603200529 ) ) ;
#2491 = DIRECTION ( 'NONE',  ( -0.9999836672264332815, 0.005715354789860036498, 0.000000000000000000 ) ) ;
#2492 = CARTESIAN_POINT ( 'NONE',  ( -105.7473861751082040, -118.0666774205683822, 3.999999999999881428 ) ) ;
#2493 = ADVANCED_FACE ( 'NONE', ( #7150 ), #1987, .F. ) ;
#2494 = CARTESIAN_POINT ( 'NONE',  ( -5.563801105733269914, -63.69014839564722763, 1.341242183458755344 ) ) ;
#2495 = CARTESIAN_POINT ( 'NONE',  ( 4.396896920912054973, -63.41639021975223045, -3.266830536337445245 ) ) ;
#2496 = CARTESIAN_POINT ( 'NONE',  ( 5.661113010068490325, -57.37064013373739613, 2.401523511004880262 ) ) ;
#2497 = CARTESIAN_POINT ( 'NONE',  ( 4.860610968486169803, 1.172374092613760688, 3.000000000000000000 ) ) ;
#2498 = ORIENTED_EDGE ( 'NONE', *, *, #3695, .T. ) ;
#2499 = B_SPLINE_CURVE_WITH_KNOTS ( 'NONE', 3,
 ( #3937, #6284, #6876, #521 ),
 .UNSPECIFIED., .F., .F.,
 ( 4, 4 ),
 ( 0.000000000000000000, 1.000000000000000000 ),
 .UNSPECIFIED. ) ;
#2500 = EDGE_LOOP ( 'NONE', ( #3703, #5611 ) ) ;
#2501 = ORIENTED_EDGE ( 'NONE', *, *, #4079, .T. ) ;
#2502 = CYLINDRICAL_SURFACE ( 'NONE', #1464, 5.000000000000001776 ) ;
#2503 = PLANE ( 'NONE',  #746 ) ;
#2504 = EDGE_CURVE ( 'NONE', #3816, #2053, #4360, .T. ) ;
#2505 = CARTESIAN_POINT ( 'NONE',  ( -1.503553670228684913, -55.21328561235763743, -1.985649781529471802 ) ) ;
#2506 = ORIENTED_EDGE ( 'NONE', *, *, #3456, .F. ) ;
#2507 = EDGE_LOOP ( 'NONE', ( #810, #2686, #1731, #5231 ) ) ;
#2508 = EDGE_LOOP ( 'NONE', ( #6079, #3187, #2962, #2387 ) ) ;
#2509 = ORIENTED_EDGE ( 'NONE', *, *, #5359, .F. ) ;
#2510 = CARTESIAN_POINT ( 'NONE',  ( -28.32684271132307074, 12.56450996214350191, -1.493845543551522992 ) ) ;
#2511 = EDGE_CURVE ( 'NONE', #3571, #4283, #6285, .T. ) ;
#2512 = CARTESIAN_POINT ( 'NONE',  ( 14.07443455944474131, -37.03272609524245240, -0.9950371902099899302 ) ) ;
#2513 = CARTESIAN_POINT ( 'NONE',  ( 5.228045628684117041, -62.14238301185224600, -1.625324146853510232 ) ) ;
#2514 = CARTESIAN_POINT ( 'NONE',  ( 6.075450823322679383, -63.85990335785957228, 0.5148622082158803570 ) ) ;
#2515 = ORIENTED_EDGE ( 'NONE', *, *, #1153, .F. ) ;
#2516 = AXIS2_PLACEMENT_3D ( 'NONE', #4827, #2378, #230 ) ;
#2517 = ORIENTED_EDGE ( 'NONE', *, *, #5847, .T. ) ;
#2518 = DIRECTION ( 'NONE',  ( -0.005715354789845003385, -0.9999836672264335036, -1.000000000000000472E-15 ) ) ;
#2519 = CARTESIAN_POINT ( 'NONE',  ( -5.101403815575769940, -63.43555091703197490, 1.460123530859765317 ) ) ;
#2520 = VECTOR ( 'NONE', #5523, 1000.000000000000000 ) ;
#2521 = EDGE_CURVE ( 'NONE', #1697, #5807, #3415, .T. ) ;
#2522 = LINE ( 'NONE', #3609, #2144 ) ;
#2523 = CARTESIAN_POINT ( 'NONE',  ( 2.167449936104646646, -65.91963042757416247, -3.186153502388756831 ) ) ;
#2524 = VECTOR ( 'NONE', #6152, 1000.000000000000114 ) ;
#2525 = ORIENTED_EDGE ( 'NONE', *, *, #536, .T. ) ;
#2526 = CARTESIAN_POINT ( 'NONE',  ( 27.09727426766168534, -34.56548687730422387, -0.4458683620789745672 ) ) ;
#2527 = AXIS2_PLACEMENT_3D ( 'NONE', #6319, #5642, #3407 ) ;
#2528 = CARTESIAN_POINT ( 'NONE',  ( 22.93267937958154690, 20.84152453766645507, -1.493845543551514332 ) ) ;
#2529 = DIRECTION ( 'NONE',  ( 0.8688689365825387201, 0.4950421911735688463, 4.999999999999993486E-16 ) ) ;
#2530 = CARTESIAN_POINT ( 'NONE',  ( 1.402950248545461909, -54.15620739517822813, 0.01614447287717020105 ) ) ;
#2531 = CARTESIAN_POINT ( 'NONE',  ( -5.971666637568279867, -56.84728173661435591, 1.574849794282134896 ) ) ;
#2532 = CARTESIAN_POINT ( 'NONE',  ( 4.860610968486169803, 1.172374092613760688, -17.67054229618195293 ) ) ;
#2533 = ORIENTED_EDGE ( 'NONE', *, *, #4904, .F. ) ;
#2534 = ORIENTED_EDGE ( 'NONE', *, *, #2721, .F. ) ;
#2535 = AXIS2_PLACEMENT_3D ( 'NONE', #1480, #4950, #3771 ) ;
#2536 = EDGE_CURVE ( 'NONE', #6689, #138, #993, .T. ) ;
#2537 = DIRECTION ( 'NONE',  ( 0.3128463504745289669, 0.9445772445362837777, 0.09950371902099887367 ) ) ;
#2538 = CARTESIAN_POINT ( 'NONE',  ( -12.10129460565897475, -12.45149060151658027, -3.000000000000013323 ) ) ;
#2539 = CARTESIAN_POINT ( 'NONE',  ( -5.010373352768399791, -62.05347898811812968, 1.680690861613699516 ) ) ;
#2540 = CARTESIAN_POINT ( 'NONE',  ( 0.5703416102740482829, -66.66371095433655114, 3.059999667144134960 ) ) ;
#2541 = ORIENTED_EDGE ( 'NONE', *, *, #6003, .F. ) ;
#2542 = VERTEX_POINT ( 'NONE', #1796 ) ;
#2543 = ORIENTED_EDGE ( 'NONE', *, *, #4264, .F. ) ;
#2544 = APPLICATION_CONTEXT ( 'automotive_design' ) ;
#2545 = ADVANCED_FACE ( 'NONE', ( #1085 ), #4024, .F. ) ;
#2546 = EDGE_CURVE ( 'NONE', #7283, #1547, #3978, .T. ) ;
#2547 = AXIS2_PLACEMENT_3D ( 'NONE', #3845, #921, #992 ) ;
#2548 = FACE_OUTER_BOUND ( 'NONE', #1741, .T. ) ;
#2549 = DIRECTION ( 'NONE',  ( 0.3128416502900970286, -0.9445788350777319931, 0.09950339776592319330 ) ) ;
#2550 = DIRECTION ( 'NONE',  ( -5.715354789845005112E-18, -9.999836672264339449E-16, 1.000000000000000000 ) ) ;
#2551 = CARTESIAN_POINT ( 'NONE',  ( -1.892846266465454841, -54.28526762408564110, -0.1610563749503846620 ) ) ;
#2552 = ORIENTED_EDGE ( 'NONE', *, *, #4764, .F. ) ;
#2553 = MECHANICAL_DESIGN_GEOMETRIC_PRESENTATION_REPRESENTATION (  '', ( #863 ), #3627 ) ;
#2554 = B_SPLINE_CURVE_WITH_KNOTS ( 'NONE', 3,
 ( #2351, #2267, #2413, #6862, #547, #2831, #1785, #1188, #6943, #2977, #1225, #3508, #3470, #1706, #5828, #658, #2945, #124, #5260 ),
 .UNSPECIFIED., .F., .F.,
 ( 4, 2, 2, 2, 2, 1, 2, 2, 2, 4 ),
 ( 0.000000000000000000, 0.1250000000000031641, 0.2500000000000063283, 0.3750000000000094924, 0.4375000000000104916, 0.4687500000000099920, 0.4843750000000104361, 0.5000000000000108802, 0.7500000000000054401, 1.000000000000000000 ),
 .UNSPECIFIED. ) ;
#2555 = AXIS2_PLACEMENT_3D ( 'NONE', #2668, #4975, #6333 ) ;
#2556 = EDGE_CURVE ( 'NONE', #1441, #6014, #2436, .T. ) ;
#2557 = FILL_AREA_STYLE_COLOUR ( '', #4966 ) ;
#2558 = VECTOR ( 'NONE', #1037, 999.9999999999998863 ) ;
#2559 = CARTESIAN_POINT ( 'NONE',  ( 5.661089107917369745, -62.15448909529578003, 2.785446686898291002 ) ) ;
#2560 = AXIS2_PLACEMENT_3D ( 'NONE', #3482, #5074, #4022 ) ;
#2561 = DIRECTION ( 'NONE',  ( 5.715354789845005112E-18, 9.999836672264339449E-16, -1.000000000000000000 ) ) ;
#2562 = DIRECTION ( 'NONE',  ( 0.9999836672264332815, -0.005715354789845002517, 0.000000000000000000 ) ) ;
#2563 = CARTESIAN_POINT ( 'NONE',  ( -3.419625075451274920, -55.70566946813526954, -0.1180528406916061396 ) ) ;
#2564 = VECTOR ( 'NONE', #6276, 1000.000000000000000 ) ;
#2565 = CIRCLE ( 'NONE', #6750, 0.7500000000000000000 ) ;
#2566 = ORIENTED_EDGE ( 'NONE', *, *, #1733, .F. ) ;
#2567 = CIRCLE ( 'NONE', #3884, 1.000000000000000000 ) ;
#2568 = DIRECTION ( 'NONE',  ( 5.715354789845005112E-18, 9.999836672264339449E-16, -1.000000000000000000 ) ) ;
#2569 = AXIS2_PLACEMENT_3D ( 'NONE', #1683, #1646, #7363 ) ;
#2570 = DIRECTION ( 'NONE',  ( -5.715354789860003484E-18, -9.999836672264337477E-16, 1.000000000000000000 ) ) ;
#2571 = FACE_OUTER_BOUND ( 'NONE', #3843, .T. ) ;
#2572 = DIRECTION ( 'NONE',  ( -0.5923994712829191434, -0.8056443796264689539, -8.090169943749487521E-16 ) ) ;
#2573 = CARTESIAN_POINT ( 'NONE',  ( 3.059030343303239974, -54.77303090793805040, 0.1039292770420399137 ) ) ;
#2574 = CIRCLE ( 'NONE', #774, 2.249999999999962252 ) ;
#2575 = CARTESIAN_POINT ( 'NONE',  ( -3.132958547045754827, -66.67000521241658362, -1.075502346145061683 ) ) ;
#2576 = DIRECTION ( 'NONE',  ( -0.9999836672264333925, 0.005715354789844970425, 0.000000000000000000 ) ) ;
#2577 = ORIENTED_EDGE ( 'NONE', *, *, #3180, .T. ) ;
#2578 = ORIENTED_EDGE ( 'NONE', *, *, #6874, .F. ) ;
#2579 = AXIS2_PLACEMENT_3D ( 'NONE', #6612, #6074, #5540 ) ;
#2580 = CARTESIAN_POINT ( 'NONE',  ( -15.49899450467540163, -35.75040780681265318, -2.566271404894997499 ) ) ;
#2581 = DIRECTION ( 'NONE',  ( 5.715354789845005112E-18, 9.999836672264339449E-16, -1.000000000000000000 ) ) ;
#2582 = CARTESIAN_POINT ( 'NONE',  ( -4.132930949989339631, -63.16624423302310021, 2.163545901557570428 ) ) ;
#2583 = ADVANCED_FACE ( 'NONE', ( #1680 ), #5271, .F. ) ;
#2584 = CARTESIAN_POINT ( 'NONE',  ( 5.080240932704482404, -56.71201383481658809, 0.2543090620532720836 ) ) ;
#2585 = ORIENTED_EDGE ( 'NONE', *, *, #1569, .F. ) ;
#2586 = ORIENTED_EDGE ( 'NONE', *, *, #4208, .T. ) ;
#2587 = ORIENTED_EDGE ( 'NONE', *, *, #5324, .F. ) ;
#2588 = ORIENTED_EDGE ( 'NONE', *, *, #4065, .T. ) ;
#2589 = DIRECTION ( 'NONE',  ( -0.5144810339903909124, 0.8512598437243096283, -0.1032760578577736621 ) ) ;
#2590 = DIRECTION ( 'NONE',  ( -0.9721221936972339606, -0.2344748185227520376, 0.000000000000000000 ) ) ;
#2591 = CARTESIAN_POINT ( 'NONE',  ( 19.34585819626726533, -40.86123582061801329, 2.999999999999959144 ) ) ;
#2592 = CARTESIAN_POINT ( 'NONE',  ( -3.773574383489684880, -54.58470482469731877, -0.3679774332281250393 ) ) ;
#2593 = DIRECTION ( 'NONE',  ( 0.3144019573014853464, -0.9492899500389726519, -7.355227538141627568E-16 ) ) ;
#2594 = CARTESIAN_POINT ( 'NONE',  ( -4.596296085628660322, -63.12536419624139938, 1.105086706205665070 ) ) ;
#2595 = ORIENTED_EDGE ( 'NONE', *, *, #161, .F. ) ;
#2596 = CARTESIAN_POINT ( 'NONE',  ( 0.000000000000000000, 0.000000000000000000, 3.500000000000000000 ) ) ;
#2597 = ADVANCED_FACE ( 'NONE', ( #1725 ), #101, .T. ) ;
#2598 = EDGE_CURVE ( 'NONE', #7172, #7317, #6818, .T. ) ;
#2599 = CARTESIAN_POINT ( 'NONE',  ( 1.408436980921016657, -54.83301260727528614, -1.927461220960678512 ) ) ;
#2600 = EDGE_LOOP ( 'NONE', ( #98, #3783 ) ) ;
#2601 = DIRECTION ( 'NONE',  ( -0.005715354789845003385, -0.9999836672264335036, -1.000000000000000472E-15 ) ) ;
#2602 = CARTESIAN_POINT ( 'NONE',  ( 9.311407240687648468, -51.41373841511900622, -2.502481404895003259 ) ) ;
#2603 = DIRECTION ( 'NONE',  ( 0.3128416502900974727, -0.9445788350777317710, 0.09950339776592416474 ) ) ;
#2604 = PRODUCT_DEFINITION_CONTEXT ( 'detailed design', #2150, 'design' ) ;
#2605 = EDGE_CURVE ( 'NONE', #1143, #7415, #5328, .T. ) ;
#2606 = CARTESIAN_POINT ( 'NONE',  ( 1.316624512147740012, -66.75104842734066324, 3.019790780136459851 ) ) ;
#2607 = FACE_BOUND ( 'NONE', #4450, .T. ) ;
#2608 = CARTESIAN_POINT ( 'NONE',  ( -2.296719424894785089, -67.41321183710302023, 2.506665444375390184 ) ) ;
#2609 = DIRECTION ( 'NONE',  ( -6.548793834854970868E-18, -1.145805836327743954E-15, -1.000000000000000000 ) ) ;
#2610 = ORIENTED_EDGE ( 'NONE', *, *, #2167, .F. ) ;
#2611 = VERTEX_POINT ( 'NONE', #5161 ) ;
#2612 = EDGE_LOOP ( 'NONE', ( #2105, #1042, #1732, #831 ) ) ;
#2613 = CARTESIAN_POINT ( 'NONE',  ( -13.76286933773225130, 13.32929763200878881, -0.3999035282155013471 ) ) ;
#2614 = CARTESIAN_POINT ( 'NONE',  ( 10.07902270299396008, 17.77910117033601978, 2.236547809770395911 ) ) ;
#2615 = CARTESIAN_POINT ( 'NONE',  ( -1.180326523133921945, -55.13093161118004559, 0.1348352173942452270 ) ) ;
#2616 = LINE ( 'NONE', #3290, #4231 ) ;
#2617 = CARTESIAN_POINT ( 'NONE',  ( 2.938012310013605966, -66.01711806483515943, 2.928912350400478370 ) ) ;
#2618 = VERTEX_POINT ( 'NONE', #6326 ) ;
#2619 = ORIENTED_EDGE ( 'NONE', *, *, #7361, .F. ) ;
#2620 = VERTEX_POINT ( 'NONE', #523 ) ;
#2621 = ORIENTED_EDGE ( 'NONE', *, *, #6248, .T. ) ;
#2622 = CARTESIAN_POINT ( 'NONE',  ( 27.30483170388656333, -34.44723004512044895, -3.427979277949995323E-14 ) ) ;
#2623 = DIRECTION ( 'NONE',  ( -5.715354789845005112E-18, -9.999836672264339449E-16, 1.000000000000000000 ) ) ;
#2624 = CARTESIAN_POINT ( 'NONE',  ( -22.85595574130830698, 4.627890847941666053, 0.4060579846639992274 ) ) ;
#2625 = CARTESIAN_POINT ( 'NONE',  ( -1.318626809553760104, -67.28799943462540512, -1.163043645407473958 ) ) ;
#2626 = ORIENTED_EDGE ( 'NONE', *, *, #5743, .T. ) ;
#2627 = EDGE_LOOP ( 'NONE', ( #4810, #5233, #1717, #45 ) ) ;
#2628 = EDGE_CURVE ( 'NONE', #2388, #4165, #5455, .T. ) ;
#2629 = DIRECTION ( 'NONE',  ( -5.715354789845005112E-18, -9.999836672264339449E-16, 1.000000000000000000 ) ) ;
#2630 = CARTESIAN_POINT ( 'NONE',  ( -3.156642594714314853, -54.82761582543010093, 1.871643660998590697 ) ) ;
#2631 = EDGE_LOOP ( 'NONE', ( #5850, #1408, #5648, #7101 ) ) ;
#2632 = DIRECTION ( 'NONE',  ( 0.000000000000000000, 0.000000000000000000, -1.000000000000000000 ) ) ;
#2633 = CARTESIAN_POINT ( 'NONE',  ( 12.99837876291259064, -32.41640519645540053, -3.252606517456513302E-14 ) ) ;
#2634 = ORIENTED_EDGE ( 'NONE', *, *, #2695, .F. ) ;
#2635 = ADVANCED_FACE ( 'NONE', ( #7437 ), #1166, .T. ) ;
#2636 = EDGE_CURVE ( 'NONE', #5945, #4029, #3450, .T. ) ;
#2637 = DIRECTION ( 'NONE',  ( -0.9999836672264333925, 0.005715354789844476896, 0.000000000000000000 ) ) ;
#2638 = CYLINDRICAL_SURFACE ( 'NONE', #4386, 0.7499999999999997780 ) ;
#2639 = DIRECTION ( 'NONE',  ( 0.6713653717953970146, -0.7411265327553913096, -7.372773368101209313E-16 ) ) ;
#2640 = CARTESIAN_POINT ( 'NONE',  ( -25.53008038988497930, -12.83396994533167756, -1.301042606982605321E-14 ) ) ;
#2641 = CARTESIAN_POINT ( 'NONE',  ( -16.40387102536037744, 1.778486824056636939, 3.000000000000001776 ) ) ;
#2642 = CARTESIAN_POINT ( 'NONE',  ( 3.318166867071405068, -54.31318850506334428, -0.01554017946999016950 ) ) ;
#2643 = CARTESIAN_POINT ( 'NONE',  ( -14.38395162568180652, 6.352317343304404673, 6.071532165918824830E-15 ) ) ;
#2644 = EDGE_LOOP ( 'NONE', ( #5023, #5527 ) ) ;
#2645 = CARTESIAN_POINT ( 'NONE',  ( -19.02833027023232404, 14.48681530925147776, 0.1446440811472397281 ) ) ;
#2646 = EDGE_CURVE ( 'NONE', #2710, #75, #26, .T. ) ;
#2647 = AXIS2_PLACEMENT_3D ( 'NONE', #96, #1823, #6427 ) ;
#2648 = CYLINDRICAL_SURFACE ( 'NONE', #6186, 11.50000000000000178 ) ;
#2649 = CARTESIAN_POINT ( 'NONE',  ( 21.92563132188844932, 21.95321433679954026, -1.493845543551513444 ) ) ;
#2650 = CARTESIAN_POINT ( 'NONE',  ( 2.959376181595404720, -55.87711464508088710, 0.4000749283577051951 ) ) ;
#2651 = DIRECTION ( 'NONE',  ( -0.9721221936972339606, -0.2344748185227520099, 0.000000000000000000 ) ) ;
#2652 = CARTESIAN_POINT ( 'NONE',  ( 5.623883274648896702, -63.28098278875869909, 0.6212483640015137309 ) ) ;
#2653 = ORIENTED_EDGE ( 'NONE', *, *, #4815, .T. ) ;
#2654 = AXIS2_PLACEMENT_3D ( 'NONE', #506, #6127, #5633 ) ;
#2655 = CARTESIAN_POINT ( 'NONE',  ( -5.707180516281660232, -57.33854382299282548, -2.489482313002657321 ) ) ;
#2656 = ORIENTED_EDGE ( 'NONE', *, *, #2546, .F. ) ;
#2657 = ORIENTED_EDGE ( 'NONE', *, *, #1351, .T. ) ;
#2658 = ORIENTED_EDGE ( 'NONE', *, *, #6680, .F. ) ;
#2659 = DIRECTION ( 'NONE',  ( 1.000000000000000000, 0.000000000000000000, 0.000000000000000000 ) ) ;
#2660 = CARTESIAN_POINT ( 'NONE',  ( -19.13960539129976368, 14.35165484499600375, -2.993845543551525878 ) ) ;
#2661 = CIRCLE ( 'NONE', #1239, 2.500000000000000000 ) ;
#2662 = CARTESIAN_POINT ( 'NONE',  ( -14.07431766324680034, -37.03265636863024923, 1.026284428608169819 ) ) ;
#2663 = LINE ( 'NONE', #3374, #4610 ) ;
#2664 = CARTESIAN_POINT ( 'NONE',  ( 5.676184037656430093, -63.13711808556965366, -1.485967351095627720 ) ) ;
#2665 = VERTEX_POINT ( 'NONE', #6924 ) ;
#2666 = AXIS2_PLACEMENT_3D ( 'NONE', #1296, #3084, #6479 ) ;
#2667 = PLANE ( 'NONE',  #34 ) ;
#2668 = CARTESIAN_POINT ( 'NONE',  ( 24.80820526761568345, 22.47304504285837368, -8.815182418718737978 ) ) ;
#2669 = CIRCLE ( 'NONE', #6633, 0.7499999999999872324 ) ;
#2670 = AXIS2_PLACEMENT_3D ( 'NONE', #5581, #4301, #4157 ) ;
#2671 = DIRECTION ( 'NONE',  ( 0.9492883822130743221, -0.3144066910790611069, 0.000000000000000000 ) ) ;
#2672 = CARTESIAN_POINT ( 'NONE',  ( 18.04796579205319063, 16.34913706177017190, 3.306154456448483714 ) ) ;
#2673 = AXIS2_PLACEMENT_3D ( 'NONE', #2946, #6509, #3473 ) ;
#2674 = EDGE_CURVE ( 'NONE', #4811, #5242, #4058, .T. ) ;
#2675 = ORIENTED_EDGE ( 'NONE', *, *, #943, .F. ) ;
#2676 = AXIS2_PLACEMENT_3D ( 'NONE', #4426, #2085, #995 ) ;
#2677 = CARTESIAN_POINT ( 'NONE',  ( 11.65361085287446663, 10.55667343862480578, 1.040834085586084257E-14 ) ) ;
#2678 = UNCERTAINTY_MEASURE_WITH_UNIT (LENGTH_MEASURE( 1.000000000000000082E-05 ), #2346, 'distance_accuracy_value', 'NONE');
#2679 = LINE ( 'NONE', #6124, #2520 ) ;
#2680 = CARTESIAN_POINT ( 'NONE',  ( -12.80424950550273167, -30.40040925781620729, -3.047309356355731468E-14 ) ) ;
#2681 = VECTOR ( 'NONE', #1084, 1000.000000000000000 ) ;
#2682 = CARTESIAN_POINT ( 'NONE',  ( 3.691078954254495059, -54.53160935192415337, 2.105200478230089267 ) ) ;
#2683 = EDGE_CURVE ( 'NONE', #7093, #3534, #5218, .T. ) ;
#2684 = CARTESIAN_POINT ( 'NONE',  ( 27.55235279947333993, -34.88166451341173513, 2.999999999999965361 ) ) ;
#2685 = AXIS2_PLACEMENT_3D ( 'NONE', #5963, #782, #3145 ) ;
#2686 = ORIENTED_EDGE ( 'NONE', *, *, #609, .F. ) ;
#2687 = FACE_OUTER_BOUND ( 'NONE', #891, .T. ) ;
#2688 = AXIS2_PLACEMENT_3D ( 'NONE', #5173, #2179, #541 ) ;
#2689 = CARTESIAN_POINT ( 'NONE',  ( -45.28625779897078729, -94.36209361619114588, -3.001000000000095813 ) ) ;
#2690 = AXIS2_PLACEMENT_3D ( 'NONE', #5976, #4797, #1331 ) ;
#2691 = AXIS2_PLACEMENT_3D ( 'NONE', #6675, #4775, #1309 ) ;
#2692 = FACE_BOUND ( 'NONE', #5121, .T. ) ;
#2693 = CARTESIAN_POINT ( 'NONE',  ( 2.837825173909910514, -64.65273986048342181, -2.563810374748431098 ) ) ;
#2694 = CARTESIAN_POINT ( 'NONE',  ( 27.99155020480830913, -34.64269665124812292, 3.130807245034128883 ) ) ;
#2695 = EDGE_CURVE ( 'NONE', #6347, #7087, #1925, .T. ) ;
#2696 = PLANE ( 'NONE',  #4823 ) ;
#2697 = EDGE_CURVE ( 'NONE', #7434, #3587, #1944, .T. ) ;
#2698 = VERTEX_POINT ( 'NONE', #214 ) ;
#2699 = AXIS2_PLACEMENT_3D ( 'NONE', #2602, #4912, #6451 ) ;
#2700 = ORIENTED_EDGE ( 'NONE', *, *, #1988, .T. ) ;
#2701 = EDGE_LOOP ( 'NONE', ( #2266, #5296, #5800, #6705 ) ) ;
#2702 = DIRECTION ( 'NONE',  ( 0.000000000000000000, 0.000000000000000000, 1.000000000000000000 ) ) ;
#2703 = CARTESIAN_POINT ( 'NONE',  ( 39.48483786921892857, -95.33781693134928048, -1.000000000000095035 ) ) ;
#2704 = CARTESIAN_POINT ( 'NONE',  ( -17.66408190574286508, 13.97695476434122952, -2.479608496603234791 ) ) ;
#2705 = CARTESIAN_POINT ( 'NONE',  ( 22.42915535073499811, 21.39736943723299945, -1.493845543551999944 ) ) ;
#2706 = CARTESIAN_POINT ( 'NONE',  ( -6.728394430327000464, -62.68905628767773663, 2.815217869383099814 ) ) ;
#2707 = DIRECTION ( 'NONE',  ( -0.9793199139485103677, -0.2023178344681514362, -2.079116908177635377E-16 ) ) ;
#2708 = DIRECTION ( 'NONE',  ( -0.2467992669038191755, 0.02032136184815236737, 0.9688535307818070264 ) ) ;
#2709 = CARTESIAN_POINT ( 'NONE',  ( -2.642495264810874822, -65.73545435749777255, -0.8365618114303696728 ) ) ;
#2710 = VERTEX_POINT ( 'NONE', #1411 ) ;
#2711 = CARTESIAN_POINT ( 'NONE',  ( 3.603225912324908187, 20.45020204625077298, -3.299999999999978950 ) ) ;
#2712 = CARTESIAN_POINT ( 'NONE',  ( -6.020862807469525180, -62.43680103905647627, 1.595792085579407216 ) ) ;
#2713 = VERTEX_POINT ( 'NONE', #134 ) ;
#2714 = CARTESIAN_POINT ( 'NONE',  ( 18.74668230531430879, -39.89873697698326538, 3.499999999999960032 ) ) ;
#2715 = LINE ( 'NONE', #2640, #2998 ) ;
#2716 = CARTESIAN_POINT ( 'NONE',  ( -6.177019684192219806, -63.92521542081036756, -0.3671906505365997164 ) ) ;
#2717 = CARTESIAN_POINT ( 'NONE',  ( 14.63763862841553376, 20.11382921380832656, -0.9938455435515094472 ) ) ;
#2718 = EDGE_LOOP ( 'NONE', ( #7164, #1311, #5601, #2412 ) ) ;
#2719 = DIRECTION ( 'NONE',  ( 2.290931512739800066E-16, 1.403768413105889815E-16, 1.000000000000000000 ) ) ;
#2720 = CARTESIAN_POINT ( 'NONE',  ( -1.308638315835680022, -65.34704488060808103, -0.1780822347184347620 ) ) ;
#2721 = EDGE_CURVE ( 'NONE', #4944, #7318, #3400, .T. ) ;
#2722 = CARTESIAN_POINT ( 'NONE',  ( 15.39900769062488806, 3.181283097128403625, 3.269241930315631824E-15 ) ) ;
#2723 = DIRECTION ( 'NONE',  ( -0.02358931830619094214, 0.9997217333147506713, 9.995705837626806266E-16 ) ) ;
#2724 = CARTESIAN_POINT ( 'NONE',  ( 4.676675357529780364, -57.90541686953501710, 2.165367849443769810 ) ) ;
#2725 = CYLINDRICAL_SURFACE ( 'NONE', #3260, 2.249999999999996891 ) ;
#2726 = DIRECTION ( 'NONE',  ( -5.715354789845005112E-18, -9.999836672264339449E-16, 1.000000000000000000 ) ) ;
#2727 = ORIENTED_EDGE ( 'NONE', *, *, #3679, .F. ) ;
#2728 = VERTEX_POINT ( 'NONE', #5986 ) ;
#2729 = APPLICATION_PROTOCOL_DEFINITION ( 'draft international standard', 'automotive_design', 1998, #2150 ) ;
#2730 = EDGE_CURVE ( 'NONE', #2713, #7422, #3272, .T. ) ;
#2731 = CARTESIAN_POINT ( 'NONE',  ( -20.16480223318149356, 14.61937842657788167, 0.006154456448484012937 ) ) ;
#2732 = ORIENTED_EDGE ( 'NONE', *, *, #707, .F. ) ;
#2733 = DIRECTION ( 'NONE',  ( -5.715354789845005112E-18, -9.999836672264339449E-16, 1.000000000000000000 ) ) ;
#2734 = CARTESIAN_POINT ( 'NONE',  ( 6.939112688521190009, -58.99009576954022549, 0.7806222117286002460 ) ) ;
#2735 = DIRECTION ( 'NONE',  ( -0.9999836672264332815, 0.005715354789860036498, 0.000000000000000000 ) ) ;
#2736 = DIRECTION ( 'NONE',  ( -0.8474369140690223290, 0.5308961072311346729, 5.260440335992993929E-16 ) ) ;
#2737 = EDGE_CURVE ( 'NONE', #7172, #1441, #3095, .T. ) ;
#2738 = CARTESIAN_POINT ( 'NONE',  ( 1.785462125252589960, -54.25404267560509908, 2.136629312307830375 ) ) ;
#2739 = CYLINDRICAL_SURFACE ( 'NONE', #7204, 2.500000000000000000 ) ;
#2740 = CARTESIAN_POINT ( 'NONE',  ( 1.714606436958001585E-17, 2.999951001679301835E-15, -3.000000000000000888 ) ) ;
#2741 = EDGE_LOOP ( 'NONE', ( #2048, #131, #5871, #2091 ) ) ;
#2742 = CARTESIAN_POINT ( 'NONE',  ( 17.91123389404125277, -40.39877837690324469, 3.263394571671051292 ) ) ;
#2743 = DIRECTION ( 'NONE',  ( -1.602374898470634869E-16, 1.442524254523139935E-17, 1.000000000000000000 ) ) ;
#2744 = CARTESIAN_POINT ( 'NONE',  ( 6.134453413605339911, -63.99854120705014537, -1.074823505768055742 ) ) ;
#2745 = CARTESIAN_POINT ( 'NONE',  ( 15.08188723176695056, -33.26566631243199623, 4.383914193272020476 ) ) ;
#2746 = AXIS2_PLACEMENT_3D ( 'NONE', #6413, #5317, #3544 ) ;
#2747 = ORIENTED_EDGE ( 'NONE', *, *, #4402, .F. ) ;
#2748 = DIRECTION ( 'NONE',  ( 0.9147661038495488173, -0.4039838799357178822, 0.000000000000000000 ) ) ;
#2749 = CARTESIAN_POINT ( 'NONE',  ( -5.038070929474960380, -61.61169989543196834, 3.303768584289609844 ) ) ;
#2750 = DIRECTION ( 'NONE',  ( -0.9147661038495488173, 0.4039838799357178822, 0.000000000000000000 ) ) ;
#2751 = CIRCLE ( 'NONE', #357, 147.0000000000000284 ) ;
#2752 = CYLINDRICAL_SURFACE ( 'NONE', #2191, 4.000000000000000000 ) ;
#2753 = CARTESIAN_POINT ( 'NONE',  ( -1.429016193381374089, -55.57463605963037168, -1.413872718151093721 ) ) ;
#2754 = CARTESIAN_POINT ( 'NONE',  ( 18.27182554301009532, -39.59382808135931242, -0.4457246814534224222 ) ) ;
#2755 = CARTESIAN_POINT ( 'NONE',  ( 35.29520910885068474, 7.091311828723104504, -1.944871132915119150 ) ) ;
#2756 = ORIENTED_EDGE ( 'NONE', *, *, #226, .F. ) ;
#2757 = ADVANCED_FACE ( 'NONE', ( #5874 ), #178, .T. ) ;
#2758 = ORIENTED_EDGE ( 'NONE', *, *, #1053, .T. ) ;
#2759 = ORIENTED_EDGE ( 'NONE', *, *, #4905, .F. ) ;
#2760 = AXIS2_PLACEMENT_3D ( 'NONE', #5519, #341, #1022 ) ;
#2761 = DIRECTION ( 'NONE',  ( -5.715354789845005112E-18, -9.999836672264339449E-16, 1.000000000000000000 ) ) ;
#2762 = DIRECTION ( 'NONE',  ( -5.715354789860003484E-18, -9.999836672264337477E-16, 1.000000000000000000 ) ) ;
#2763 = CARTESIAN_POINT ( 'NONE',  ( -43.04083572346265640, -94.50554989113550164, -3.000000000000095479 ) ) ;
#2764 = AXIS2_PLACEMENT_3D ( 'NONE', #3930, #4014, #4466 ) ;
#2765 = CARTESIAN_POINT ( 'NONE',  ( -32.92087242456759100, 14.53869105662955796, -2.993845543551514776 ) ) ;
#2766 = CARTESIAN_POINT ( 'NONE',  ( -6.487383171013251015, -57.01613561570176358, -1.117195879216653864 ) ) ;
#2767 = ORIENTED_EDGE ( 'NONE', *, *, #4549, .T. ) ;
#2768 = EDGE_CURVE ( 'NONE', #3946, #4056, #4237, .T. ) ;
#2769 = EDGE_CURVE ( 'NONE', #1506, #3480, #5382, .T. ) ;
#2770 = DIRECTION ( 'NONE',  ( 5.715354789860003484E-18, 9.999836672264337477E-16, -1.000000000000000000 ) ) ;
#2771 =( NAMED_UNIT ( * ) PLANE_ANGLE_UNIT ( ) SI_UNIT ( $, .RADIAN. ) );
#2772 = CARTESIAN_POINT ( 'NONE',  ( 3.059030343303239974, -54.77303090793805040, 0.1039292770420399137 ) ) ;
#2773 = DIRECTION ( 'NONE',  ( -5.715354789845005112E-18, -9.999836672264339449E-16, 1.000000000000000000 ) ) ;
#2774 = DIRECTION ( 'NONE',  ( -5.715354789845005112E-18, -9.999836672264339449E-16, 1.000000000000000000 ) ) ;
#2775 = CARTESIAN_POINT ( 'NONE',  ( 14.63724902514210058, -35.33341991383040437, 3.658178766884820465 ) ) ;
#2776 = EDGE_CURVE ( 'NONE', #1000, #3480, #5409, .T. ) ;
#2777 = ADVANCED_FACE ( 'NONE', ( #4740 ), #869, .T. ) ;
#2778 = ORIENTED_EDGE ( 'NONE', *, *, #3118, .F. ) ;
#2779 = AXIS2_PLACEMENT_3D ( 'NONE', #3235, #2570, #384 ) ;
#2780 = AXIS2_PLACEMENT_3D ( 'NONE', #6472, #5030, #2651 ) ;
#2781 = DIRECTION ( 'NONE',  ( 0.9999836672264335036, -0.005715354789845041548, 0.000000000000000000 ) ) ;
#2782 = CARTESIAN_POINT ( 'NONE',  ( -18.51952944085035924, 14.44713361607365876, 0.4060579846639944535 ) ) ;
#2783 = CARTESIAN_POINT ( 'NONE',  ( 35.25551690214635414, 7.283442040853447708, 7.484820869439482625E-15 ) ) ;
#2784 = CARTESIAN_POINT ( 'NONE',  ( 3.832282121198885338, -54.47902871778750722, 0.5155147207099053386 ) ) ;
#2785 = DIRECTION ( 'NONE',  ( 5.715354789860003484E-18, 9.999836672264337477E-16, -1.000000000000000000 ) ) ;
#2786 = CIRCLE ( 'NONE', #4486, 0.7500000000000003331 ) ;
#2787 = VECTOR ( 'NONE', #5737, 1000.000000000000114 ) ;
#2788 = VERTEX_POINT ( 'NONE', #2538 ) ;
#2789 =( GEOMETRIC_REPRESENTATION_CONTEXT ( 3 ) GLOBAL_UNCERTAINTY_ASSIGNED_CONTEXT ( ( #3056 ) ) GLOBAL_UNIT_ASSIGNED_CONTEXT ( ( #2434, #1347, #4096 ) ) REPRESENTATION_CONTEXT ( 'NONE', 'WORKASPACE' ) );
#2790 = ORIENTED_EDGE ( 'NONE', *, *, #4686, .T. ) ;
#2791 = CARTESIAN_POINT ( 'NONE',  ( 2.837825173909910514, -64.65273986048342181, -2.563810374748431098 ) ) ;
#2792 = CARTESIAN_POINT ( 'NONE',  ( -32.59768532061907109, 15.27050393970921327, -1.493845543551520327 ) ) ;
#2793 = VECTOR ( 'NONE', #5451, 1000.000000000000000 ) ;
#2794 = AXIS2_PLACEMENT_3D ( 'NONE', #4854, #2992, #221 ) ;
#2795 = LINE ( 'NONE', #7393, #5338 ) ;
#2796 = CARTESIAN_POINT ( 'NONE',  ( -2.678905510920184696, -65.04233304593640241, 0.9295552878624004922 ) ) ;
#2797 = DIRECTION ( 'NONE',  ( -0.4950421911735689018, 0.8688689365825386091, 0.000000000000000000 ) ) ;
#2798 = FACE_OUTER_BOUND ( 'NONE', #6354, .T. ) ;
#2799 = ORIENTED_EDGE ( 'NONE', *, *, #162, .F. ) ;
#2800 = VECTOR ( 'NONE', #5789, 1000.000000000000227 ) ;
#2801 = ORIENTED_EDGE ( 'NONE', *, *, #3234, .F. ) ;
#2802 = ORIENTED_EDGE ( 'NONE', *, *, #6003, .T. ) ;
#2803 = AXIS2_PLACEMENT_3D ( 'NONE', #2960, #6881, #5302 ) ;
#2804 = DIRECTION ( 'NONE',  ( -0.9999836672264333925, 0.005715354789844476896, 0.000000000000000000 ) ) ;
#2805 = ORIENTED_EDGE ( 'NONE', *, *, #2990, .F. ) ;
#2806 = ADVANCED_FACE ( 'NONE', ( #6493 ), #6065, .F. ) ;
#2807 = DIRECTION ( 'NONE',  ( -0.9999836672264333925, 0.005715354789844960016, 0.000000000000000000 ) ) ;
#2808 = CARTESIAN_POINT ( 'NONE',  ( 13.12514617723165955, -36.71831940416339535, -0.9950371902099899302 ) ) ;
#2809 = PLANE ( 'NONE',  #883 ) ;
#2810 = CARTESIAN_POINT ( 'NONE',  ( -2.296719424894785089, -67.41321183710302023, 2.506665444375390184 ) ) ;
#2811 = AXIS2_PLACEMENT_3D ( 'NONE', #4289, #5993, #6141 ) ;
#2812 = ORIENTED_EDGE ( 'NONE', *, *, #4038, .T. ) ;
#2813 = ORIENTED_EDGE ( 'NONE', *, *, #7191, .T. ) ;
#2814 = CARTESIAN_POINT ( 'NONE',  ( 7.529070345495034289, 16.11642554373086256, 1.604619215278546562E-14 ) ) ;
#2815 =( LENGTH_UNIT ( ) NAMED_UNIT ( * ) SI_UNIT ( .MILLI., .METRE. ) );
#2816 = CARTESIAN_POINT ( 'NONE',  ( -19.52657036150863235, 8.623428025244454176, -2.230393353321931560 ) ) ;
#2817 = CIRCLE ( 'NONE', #5119, 0.9999999999999998890 ) ;
#2818 = EDGE_CURVE ( 'NONE', #2276, #6322, #5906, .T. ) ;
#2819 = DIRECTION ( 'NONE',  ( 0.5194059912184716410, -0.8545275983175482093, -8.515450519919942904E-16 ) ) ;
#2820 = CARTESIAN_POINT ( 'NONE',  ( 13.49911764349216092, -35.75048010860329839, 2.597518595105000383 ) ) ;
#2821 = EDGE_LOOP ( 'NONE', ( #804, #5120, #2778, #518 ) ) ;
#2822 = ORIENTED_EDGE ( 'NONE', *, *, #1819, .F. ) ;
#2823 = EDGE_CURVE ( 'NONE', #1493, #5081, #3024, .T. ) ;
#2824 = LINE ( 'NONE', #2140, #5695 ) ;
#2825 = ADVANCED_FACE ( 'NONE', ( #6019, #1895, #1279 ), #2471, .T. ) ;
#2826 = DIRECTION ( 'NONE',  ( 0.1628827478269146978, -0.7884342920379695530, 0.5931615105508275532 ) ) ;
#2827 = CARTESIAN_POINT ( 'NONE',  ( 37.86567095459282228, 7.005780695865149177, -1.500000000001998623 ) ) ;
#2828 = CARTESIAN_POINT ( 'NONE',  ( -6.840816475388580287, -61.57127885238590892, 1.848044054229609934 ) ) ;
#2829 = DIRECTION ( 'NONE',  ( 6.276044648701490311E-18, 1.098084436444154719E-15, -1.000000000000000000 ) ) ;
#2830 = VERTEX_POINT ( 'NONE', #5951 ) ;
#2831 = CARTESIAN_POINT ( 'NONE',  ( -4.908491537261493676, -62.07009784221990856, 3.085829421542757522 ) ) ;
#2832 = CARTESIAN_POINT ( 'NONE',  ( 9.358334193258830425, -51.27205182843857045, -2.495037190209989930 ) ) ;
#2833 = CARTESIAN_POINT ( 'NONE',  ( 27.98760434640042050, 26.43260972569849443, -1.493845543551990174 ) ) ;
#2834 = CARTESIAN_POINT ( 'NONE',  ( -4.871804169514039273, -62.10086352108921659, 3.270302337133240478 ) ) ;
#2835 = DIRECTION ( 'NONE',  ( -5.715354789845005112E-18, -9.999836672264339449E-16, 1.000000000000000000 ) ) ;
#2836 = CARTESIAN_POINT ( 'NONE',  ( -5.046087304442132826, -64.12077430324966087, -0.7947617384407686947 ) ) ;
#2837 = ORIENTED_EDGE ( 'NONE', *, *, #7104, .T. ) ;
#2838 = EDGE_LOOP ( 'NONE', ( #2476, #2213 ) ) ;
#2839 = ORIENTED_EDGE ( 'NONE', *, *, #3335, .F. ) ;
#2840 = ITEM_DEFINED_TRANSFORMATION ( 'NONE', 'NONE', #4494,  #751 ) ;
#2841 = DIRECTION ( 'NONE',  ( -5.715354789845005112E-18, -9.999836672264339449E-16, 1.000000000000000000 ) ) ;
#2842 = ORIENTED_EDGE ( 'NONE', *, *, #7245, .T. ) ;
#2843 = CARTESIAN_POINT ( 'NONE',  ( -41.31559769795914150, -94.79889909491285493, -9.503348406515855143E-14 ) ) ;
#2844 = LINE ( 'NONE', #5162, #287 ) ;
#2845 = CARTESIAN_POINT ( 'NONE',  ( -7.672523287152989369, -8.566351989504937592, -8.673617379884035472E-15 ) ) ;
#2846 = CARTESIAN_POINT ( 'NONE',  ( -6.955550688080649913, -62.00810176775132021, 2.849210506046880642 ) ) ;
#2847 = EDGE_LOOP ( 'NONE', ( #5275, #4432, #6575, #2467 ) ) ;
#2848 = CARTESIAN_POINT ( 'NONE',  ( 8.041936255418978163, 16.36526498932675366, 2.068895131770362987E-14 ) ) ;
#2849 = CARTESIAN_POINT ( 'NONE',  ( 27.23321219009249816, -35.06498951359424865, -1.000000000000034861 ) ) ;
#2850 = DIRECTION ( 'NONE',  ( -5.715354789845005112E-18, -9.999836672264339449E-16, 1.000000000000000000 ) ) ;
#2851 = DIRECTION ( 'NONE',  ( 0.9999836672264332815, -0.005715354789845002517, 0.000000000000000000 ) ) ;
#2852 = CARTESIAN_POINT ( 'NONE',  ( 30.07944552268752503, 5.397223322909749932, -1.499999999999994893 ) ) ;
#2853 = LINE ( 'NONE', #4530, #2885 ) ;
#2854 = ORIENTED_EDGE ( 'NONE', *, *, #4440, .F. ) ;
#2855 = VERTEX_POINT ( 'NONE', #835 ) ;
#2856 = ADVANCED_FACE ( 'NONE', ( #776 ), #2503, .F. ) ;
#2857 = DIRECTION ( 'NONE',  ( -0.9147661038495482622, 0.4039838799357193255, 3.987490689252457863E-16 ) ) ;
#2858 = FACE_OUTER_BOUND ( 'NONE', #7280, .T. ) ;
#2859 = DIRECTION ( 'NONE',  ( 0.9999836672264332815, -0.005715354789845002517, 0.000000000000000000 ) ) ;
#2860 = CARTESIAN_POINT ( 'NONE',  ( -3.723298236168965047, -66.76642012610518861, 0.4732191326009700938 ) ) ;
#2861 = DIRECTION ( 'NONE',  ( 5.715354789845005112E-18, 9.999836672264339449E-16, -1.000000000000000000 ) ) ;
#2862 = EDGE_LOOP ( 'NONE', ( #220, #5634, #1983, #5635 ) ) ;
#2863 = EDGE_CURVE ( 'NONE', #89, #5783, #956, .T. ) ;
#2864 = ADVANCED_FACE ( 'NONE', ( #6714 ), #3247, .T. ) ;
#2865 = CARTESIAN_POINT ( 'NONE',  ( -9.311346830843410416, -51.41373841511902043, 1.533728595105000370 ) ) ;
#2866 = CARTESIAN_POINT ( 'NONE',  ( 18.52003153382460354, -40.03437257541853711, -1.000000000000039746 ) ) ;
#2867 = CARTESIAN_POINT ( 'NONE',  ( 39.32685927492619982, -94.35036853610694152, -9.410874857174178487E-14 ) ) ;
#2868 = CARTESIAN_POINT ( 'NONE',  ( 4.897692307440769888, -62.02301377339387756, -1.765793165935516829 ) ) ;
#2869 = CIRCLE ( 'NONE', #7079, 1.000000000000001776 ) ;
#2870 = CARTESIAN_POINT ( 'NONE',  ( 12.68569177933871828, -46.07971015455952113, -4.597017211338538800E-14 ) ) ;
#2871 = DIRECTION ( 'NONE',  ( 0.8056443796264692869, -0.5923994712829185882, -5.877852522924713037E-16 ) ) ;
#2872 = ORIENTED_EDGE ( 'NONE', *, *, #4593, .T. ) ;
#2873 = EDGE_CURVE ( 'NONE', #1758, #4244, #2065, .T. ) ;
#2874 = EDGE_LOOP ( 'NONE', ( #1965, #6617, #4076, #4516 ) ) ;
#2875 = ORIENTED_EDGE ( 'NONE', *, *, #836, .F. ) ;
#2876 = AXIS2_PLACEMENT_3D ( 'NONE', #6196, #504, #6782 ) ;
#2877 = CARTESIAN_POINT ( 'NONE',  ( 41.70778007397900211, -94.98992620957551480, -9.475926987523308753E-14 ) ) ;
#2878 = DIRECTION ( 'NONE',  ( 0.9999836672264332815, -0.005715354789844959149, 0.000000000000000000 ) ) ;
#2879 = CARTESIAN_POINT ( 'NONE',  ( 5.608858804484560423, -63.72364544018660126, -1.429200976399037870 ) ) ;
#2880 = PLANE ( 'NONE',  #4140 ) ;
#2881 = CARTESIAN_POINT ( 'NONE',  ( -5.294444503516980483, -61.70453834742492916, -0.3952116983248150084 ) ) ;
#2882 = VECTOR ( 'NONE', #4075, 1000.000000000000227 ) ;
#2883 = ORIENTED_EDGE ( 'NONE', *, *, #4540, .F. ) ;
#2884 = CARTESIAN_POINT ( 'NONE',  ( 35.25551690214635414, 7.283442040853447708, 7.484820869439482625E-15 ) ) ;
#2885 = VECTOR ( 'NONE', #7444, 1000.000000000000227 ) ;
#2886 = B_SPLINE_SURFACE_WITH_KNOTS ( 'NONE', 3, 3, ( 
 ( #7084, #3015, #3551, #5373, #6979, #5229, #1822, #1860, #691, #4694, #2419, #5899, #2949, #2496, #1919, #3620, #2355, #1335, #3515, #4227, #1271, #6948, #6526, #1790, #2980, #5331, #4121, #5867, #5837, #170, #4083, #6425, #95, #6385, #2384, #1229, #768, #5294, #663, #5264, #128, #4729, #3059, #6454, #1299 ),
 ( #724, #2462, #205, #388, #6676, #6159, #2076, #6564, #6049, #3770, #4274, #916, #5525, #873, #2682, #6595, #278, #5441, #2531, #2032, #6010, #3088, #829, #1404, #3692, #350, #317, #6093, #6709, #4343, #2642, #4916, #3124, #6631, #4388, #1479, #1551, #4949, #2575, #7160, #7270, #5402, #3204, #4881, #4836 ),
 ( #1436, #1999, #4307, #3727, #239, #7124, #1961, #2608, #3168, #5494, #7197, #7232, #1519, #3805, #3841, #6126, #949, #3241, #5558, #4989, #2109, #4421, #2860, #432, #4502, #3957, #3882, #1066, #8, #5060, #544, #6268, #6743, #5021, #6198, #6232, #2229, #5143, #7305, #505, #6784, #1030, #1748, #3354, #6311 ),
 ( #2828, #7420, #4613, #5667, #1105, #5632, #5175, #2298, #984, #3317, #7386, #465, #1628, #4000, #2784, #3279, #2263, #4572, #2142, #4044, #5103, #2716, #6906, #1704, #1662, #4536, #2744, #1592, #6859, #5598, #4456, #7342, #575, #2182, #3920, #5746, #6820, #3393, #5710, #1151, #3434, #1782, #2942, #685, #6477 ),
 ( #4792, #2411, #7045, #3503, #5319, #713, #4109, #154, #1326, #3007, #1185, #754, #6415, #5823, #4718, #654, #5928, #4154, #7006, #3049, #5257, #7076, #1850, #6447, #5364, #197, #2488, #6345, #3467, #5780, #608, #2896, #54, #476, #2655, #1077, #1563, #6103, #3933, #5534, #3852, #2200, #6171, #1001, #4960 ),
 ( #3292, #6687, #517, #5610, #362, #4515, #2156, #6797, #1640, #7397, #4356, #6999, #593, #4061, #632, #31, #2922, #4191, #6484, #204, #2881, #5372, #6362, #2327, #5197, #1204, #1334, #1169, #5241, #6927, #7053, #3058, #1766, #5765, #3619, #3486, #5938, #1888, #766, #5805, #4640, #73, #2495, #3453, #2461 ),
 ( #4762, #3321, #509, #7002, #4508, #85, #5817, #6204, #4461, #5636, #5671, #1666, #4683, #6747, #7390, #6236, #470, #1291, #1109, #6824, #5064, #1035, #1811, #2720, #3573, #3498, #4715, #3924, #3962, #2235, #648, #5285, #4106, #436, #6964, #3889, #3360, #2938, #1599, #5253, #2376, #2791, #116, #1070, #7346 ),
 ( #6273, #2749, #5026, #2189, #6790, #1634, #6409, #5109, #1255, #7309, #5857, #681, #4542, #2971, #1845, #2147, #4258, #4329, #5429, #5922, #2484, #2594, #708, #6000, #3043, #5313, #4183, #855, #1908, #4788, #6474, #7072, #1462, #2446, #5887, #3078, #3649, #4752, #192, #817, #1357, #4218, #2019, #7149, #262 ),
 ( #2999, #6620, #1423, #306, #149, #6510, #1393, #1322, #5968, #4902, #788, #2559, #3681, #3607, #7040, #747, #5391, #7106, #4867, #1878, #228, #2519, #5360, #4825, #1945, #3714, #7185, #1985, #4296, #6584, #6552, #3111, #6038, #3153, #5479, #5655, #3755, #1510, #2709, #940, #2102, #6771, #6149, #6082, #5047 ),
 ( #6810, #3827, #3191, #2217, #4484, #495, #905, #3795, #5013, #3227, #4411, #1619, #973, #5515, #7331, #2738, #338, #2630, #3263, #4939, #4527, #3909, #4445, #7296, #5547, #2058, #2170, #7224, #7372, #6730, #2772, #7262, #2133, #5584, #1579, #1057, #6223, #4373, #3345, #6664, #6702, #3866, #6117, #6185, #1019 ) ),
 .UNSPECIFIED., .T., .F., .F.,
 ( 4, 2, 2, 2, 4 ),
 ( 4, 3, 2, 2, 2, 2, 2, 2, 2, 2, 2, 2, 2, 2, 2, 2, 2, 2, 2, 2, 2, 4 ),
 ( 0.000000000000000000, 0.2500000000000000000, 0.5000000000000000000, 0.7500000000000000000, 1.000000000000000000 ),
 ( -0.01000000000000000021, 0.000000000000000000, 0.02628634692406570106, 0.07896140836526269191, 0.1315838524972270107, 0.1842089079736879964, 0.2368304666025229932, 0.2894621644501310098, 0.3421084969797454911, 0.3947501728568885149, 0.4473769119526340154, 0.5000000000000000000, 0.5526230880473660401, 0.6052498271431119292, 0.6578915030202550085, 0.7105378355498690457, 0.7631695333974770623, 0.8157910920263119481, 0.8684161475027730726, 0.9210385916347370028, 0.9737136530759340491, 1.000000000000000000 ),
 .UNSPECIFIED. ) ;
#2887 = CARTESIAN_POINT ( 'NONE',  ( 17.61001731287966265, -39.97089645448942719, 3.499999999999960032 ) ) ;
#2888 = DIRECTION ( 'NONE',  ( 0.9999836672264332815, -0.005715354789845002517, 0.000000000000000000 ) ) ;
#2889 = CARTESIAN_POINT ( 'NONE',  ( 27.34858876736844380, -35.00074627774458946, 3.999999999999965361 ) ) ;
#2890 = ORIENTED_EDGE ( 'NONE', *, *, #1071, .T. ) ;
#2891 = CARTESIAN_POINT ( 'NONE',  ( -105.7473861751082040, -118.0666774205683822, 2.999999999999881428 ) ) ;
#2892 = VECTOR ( 'NONE', #5670, 1000.000000000000000 ) ;
#2893 = CARTESIAN_POINT ( 'NONE',  ( 11.37011796090756555, -1.723489934710175753, -1.734723475976807094E-15 ) ) ;
#2894 = EDGE_CURVE ( 'NONE', #3657, #4478, #3174, .T. ) ;
#2895 = LINE ( 'NONE', #1104, #4577 ) ;
#2896 = CARTESIAN_POINT ( 'NONE',  ( 1.531562167974070077, -54.12800115838471271, -2.047325108518057935 ) ) ;
#2897 = CARTESIAN_POINT ( 'NONE',  ( -28.26642576027046516, -36.90973657692984489, -3.707068639042112348E-14 ) ) ;
#2898 = ORIENTED_EDGE ( 'NONE', *, *, #5554, .T. ) ;
#2899 = AXIS2_PLACEMENT_3D ( 'NONE', #4509, #4543, #3438 ) ;
#2900 = CARTESIAN_POINT ( 'NONE',  ( -28.02385480137100160, 13.25058454003099939, -1.493845543551999944 ) ) ;
#2901 = TOROIDAL_SURFACE ( 'NONE', #3023, 1.500000000000000000, 1.000000000000000000 ) ;
#2902 = DIRECTION ( 'NONE',  ( 0.000000000000000000, -0.7252570966694443788, 0.6884781359858918037 ) ) ;
#2903 = DIRECTION ( 'NONE',  ( -5.715354789860003484E-18, -9.999836672264337477E-16, 1.000000000000000000 ) ) ;
#2904 = CARTESIAN_POINT ( 'NONE',  ( -45.21893524706405287, -93.36435596057614816, -3.000000000000094591 ) ) ;
#2905 = EDGE_CURVE ( 'NONE', #6113, #3586, #1604, .T. ) ;
#2906 =( GEOMETRIC_REPRESENTATION_CONTEXT ( 3 ) GLOBAL_UNCERTAINTY_ASSIGNED_CONTEXT ( ( #5327 ) ) GLOBAL_UNIT_ASSIGNED_CONTEXT ( ( #3858, #3902, #229 ) ) REPRESENTATION_CONTEXT ( 'NONE', 'WORKASPACE' ) );
#2907 = CARTESIAN_POINT ( 'NONE',  ( -5.502354252718959948, -62.02724140920135198, 3.641858308670590016 ) ) ;
#2908 = AXIS2_PLACEMENT_3D ( 'NONE', #7069, #7097, #1315 ) ;
#2909 = DIRECTION ( 'NONE',  ( -0.4039838799357104437, -0.9147661038495520369, -1.600849619044994772E-16 ) ) ;
#2910 = CARTESIAN_POINT ( 'NONE',  ( -12.36403222600316276, 10.92614786255226811, 1.085530457744840442E-14 ) ) ;
#2911 = ORIENTED_EDGE ( 'NONE', *, *, #293, .T. ) ;
#2912 = VERTEX_POINT ( 'NONE', #5564 ) ;
#2913 = ORIENTED_EDGE ( 'NONE', *, *, #3831, .F. ) ;
#2914 = AXIS2_PLACEMENT_3D ( 'NONE', #6109, #4965, #965 ) ;
#2915 = DIRECTION ( 'NONE',  ( -0.9492899500389724299, -0.3144019573014856794, 0.000000000000000000 ) ) ;
#2916 = DIRECTION ( 'NONE',  ( -5.715354789860003484E-18, -9.999836672264337477E-16, 1.000000000000000000 ) ) ;
#2917 = DIRECTION ( 'NONE',  ( -0.005715354789845003385, -0.9999836672264335036, -2.228438827623913869E-16 ) ) ;
#2918 = ADVANCED_FACE ( 'NONE', ( #358 ), #4394, .F. ) ;
#2919 = ADVANCED_FACE ( 'NONE', ( #2692, #3810 ), #3288, .T. ) ;
#2920 = CARTESIAN_POINT ( 'NONE',  ( 3.533549941398215211, -54.99147314093924166, 0.1611374604154752754 ) ) ;
#2921 = CARTESIAN_POINT ( 'NONE',  ( 27.34640600250860487, -35.00195951109004255, -0.9740265123469552533 ) ) ;
#2922 = CARTESIAN_POINT ( 'NONE',  ( -1.180326523133921945, -55.13093161118004559, 0.1348352173942452270 ) ) ;
#2923 = AXIS2_PLACEMENT_3D ( 'NONE', #2714, #7158, #3200 ) ;
#2924 = AXIS2_PLACEMENT_3D ( 'NONE', #5873, #1828, #4130 ) ;
#2925 = ORIENTED_EDGE ( 'NONE', *, *, #7382, .F. ) ;
#2926 = CIRCLE ( 'NONE', #4982, 3.750000000000000444 ) ;
#2927 = VERTEX_POINT ( 'NONE', #2649 ) ;
#2928 = AXIS2_PLACEMENT_3D ( 'NONE', #1806, #4101, #3539 ) ;
#2929 = CARTESIAN_POINT ( 'NONE',  ( 14.29543924104632779, -35.83228874779774742, -3.556183125752454544E-14 ) ) ;
#2930 = EDGE_CURVE ( 'NONE', #106, #6689, #4956, .T. ) ;
#2931 = CARTESIAN_POINT ( 'NONE',  ( 7.529070345495034289, 16.11642554373085900, 3.000000000000015987 ) ) ;
#2932 = CIRCLE ( 'NONE', #1616, 0.9999999999999998890 ) ;
#2933 = APPLICATION_CONTEXT ( 'automotive_design' ) ;
#2934 = CARTESIAN_POINT ( 'NONE',  ( 27.98760434640042050, 26.43260972569849443, -1.493845543551990174 ) ) ;
#2935 = CARTESIAN_POINT ( 'NONE',  ( -3.235261603508409856, -66.01500717273368934, 1.164464255201294929 ) ) ;
#2936 = DIRECTION ( 'NONE',  ( 0.3144019573014853464, -0.9492899500389726519, -7.355227538141627568E-16 ) ) ;
#2937 = CIRCLE ( 'NONE', #3768, 2.500000000000000000 ) ;
#2938 = CARTESIAN_POINT ( 'NONE',  ( -4.248468832057555211, -63.21868707083201855, -2.033638508047526550 ) ) ;
#2939 = FILL_AREA_STYLE_COLOUR ( '', #7001 ) ;
#2940 = DIRECTION ( 'NONE',  ( 0.2344748185227520099, -0.9721221936972339606, 0.000000000000000000 ) ) ;
#2941 = CARTESIAN_POINT ( 'NONE',  ( 5.770703635693222644, -59.55204183230187454, 0.5638254346361636360 ) ) ;
#2942 = CARTESIAN_POINT ( 'NONE',  ( 5.742131165818880056, -64.29439030986208081, -3.151051222873450630 ) ) ;
#2943 = CARTESIAN_POINT ( 'NONE',  ( -15.08175531864075047, -33.99084820126180517, -5.041145139047909396 ) ) ;
#2944 = ORIENTED_EDGE ( 'NONE', *, *, #6642, .F. ) ;
#2945 = CARTESIAN_POINT ( 'NONE',  ( -5.616612366066321194, -62.30416043735317544, 3.536847275893812537 ) ) ;
#2946 = CARTESIAN_POINT ( 'NONE',  ( -16.56077119915742202, 1.636355435069145381, 0.006154456448471436192 ) ) ;
#2947 = CARTESIAN_POINT ( 'NONE',  ( 35.76131148831677109, 4.835142255982173509, 5.039451867604972471E-15 ) ) ;
#2948 = CARTESIAN_POINT ( 'NONE',  ( 4.689255334142830023, -62.66924379293478609, -1.721810340931042793 ) ) ;
#2949 = CARTESIAN_POINT ( 'NONE',  ( 6.285636693253979779, -59.03245517747429716, 2.489777307435960374 ) ) ;
#2950 = DIRECTION ( 'NONE',  ( 5.715354789860003484E-18, 9.999836672264337477E-16, -1.000000000000000000 ) ) ;
#2951 = EDGE_LOOP ( 'NONE', ( #3730, #4935, #1716, #2157 ) ) ;
#2952 = ORIENTED_EDGE ( 'NONE', *, *, #5378, .F. ) ;
#2953 = ORIENTED_EDGE ( 'NONE', *, *, #1499, .T. ) ;
#2954 = EDGE_LOOP ( 'NONE', ( #2251, #851, #4981, #1306 ) ) ;
#2955 = PRODUCT_DEFINITION_SHAPE ( 'NONE', 'NONE',  #7450 ) ;
#2956 = EDGE_CURVE ( 'NONE', #1033, #6355, #4994, .T. ) ;
#2957 = DIRECTION ( 'NONE',  ( 0.6513146796332659472, 0.5900073775824578037, -0.4771587602596093491 ) ) ;
#2958 = CARTESIAN_POINT ( 'NONE',  ( 7.529070345495034289, 16.11642554373085900, 2.000000000000016431 ) ) ;
#2959 = CARTESIAN_POINT ( 'NONE',  ( -6.177019684192219806, -63.92521542081036756, -0.3671906505365997164 ) ) ;
#2960 = CARTESIAN_POINT ( 'NONE',  ( 0.000000000000000000, 0.000000000000000000, -2.544444444444450060 ) ) ;
#2961 = ORIENTED_EDGE ( 'NONE', *, *, #1304, .T. ) ;
#2962 = ORIENTED_EDGE ( 'NONE', *, *, #6294, .F. ) ;
#2963 = EDGE_CURVE ( 'NONE', #6869, #3480, #3872, .T. ) ;
#2964 = ADVANCED_FACE ( 'NONE', ( #323 ), #1397, .F. ) ;
#2965 = CARTESIAN_POINT ( 'NONE',  ( -41.31559769795914150, -94.79889909491285493, -3.000000000000095923 ) ) ;
#2966 = DIRECTION ( 'NONE',  ( -0.9147661038495521479, 0.4039838799357104993, 3.987490689252507167E-16 ) ) ;
#2967 = DIRECTION ( 'NONE',  ( 0.9986925448795958005, 0.05111947575940636868, 5.682652305653510796E-17 ) ) ;
#2968 = DIRECTION ( 'NONE',  ( -0.9147661038495489283, 0.4039838799357176602, 3.987490689252441100E-16 ) ) ;
#2969 = CARTESIAN_POINT ( 'NONE',  ( 27.99155020439386732, -34.64269665048638558, 3.999999999999966249 ) ) ;
#2970 = EDGE_CURVE ( 'NONE', #3589, #3446, #4850, .T. ) ;
#2971 = CARTESIAN_POINT ( 'NONE',  ( 4.676675357529780364, -57.90541686953501710, 2.165367849443769810 ) ) ;
#2972 = CARTESIAN_POINT ( 'NONE',  ( 13.61290835672744848, 19.61678186576282812, 0.1446417891851695114 ) ) ;
#2973 = DIRECTION ( 'NONE',  ( 0.000000000000000000, 0.000000000000000000, 1.000000000000000000 ) ) ;
#2974 = CARTESIAN_POINT ( 'NONE',  ( 4.690637055356551954, -57.05217919465406595, 0.4062669221328191749 ) ) ;
#2975 = DIRECTION ( 'NONE',  ( 0.9147661038495488173, -0.4039838799357178822, 0.000000000000000000 ) ) ;
#2976 = ORIENTED_EDGE ( 'NONE', *, *, #7104, .F. ) ;
#2977 = CARTESIAN_POINT ( 'NONE',  ( -5.063240685778024108, -62.12055065899711792, 3.262469527825359261 ) ) ;
#2978 = CARTESIAN_POINT ( 'NONE',  ( 18.06432739836606416, -39.71205113188410252, -3.955074325938786408E-14 ) ) ;
#2979 = CARTESIAN_POINT ( 'NONE',  ( -0.9970853242166300978, -65.67144495878099519, -1.280490079922569802 ) ) ;
#2980 = CARTESIAN_POINT ( 'NONE',  ( 1.700848490796859958, -66.65813550864595527, 0.8993149516912349872 ) ) ;
#2981 = DIRECTION ( 'NONE',  ( 0.2223191033124283789, 0.6712482523644727195, 0.7071067811865466846 ) ) ;
#2982 = ORIENTED_EDGE ( 'NONE', *, *, #4996, .T. ) ;
#2983 = ORIENTED_EDGE ( 'NONE', *, *, #119, .F. ) ;
#2984 = ORIENTED_EDGE ( 'NONE', *, *, #4687, .T. ) ;
#2985 = LINE ( 'NONE', #4279, #7008 ) ;
#2986 = ORIENTED_EDGE ( 'NONE', *, *, #253, .F. ) ;
#2987 = DIRECTION ( 'NONE',  ( -0.9492883822130747662, 0.3144066910790599412, 0.000000000000000000 ) ) ;
#2988 = CARTESIAN_POINT ( 'NONE',  ( -5.671911954242359499, -63.61502870002530585, -0.7222274751851948116 ) ) ;
#2989 = CARTESIAN_POINT ( 'NONE',  ( 27.08917575328167615, -34.57010104422300145, -0.4368814963732711165 ) ) ;
#2990 = EDGE_CURVE ( 'NONE', #4056, #2431, #2151, .T. ) ;
#2991 = VERTEX_POINT ( 'NONE', #4463 ) ;
#2992 = DIRECTION ( 'NONE',  ( 0.9793199139485100346, 0.2023178344681531293, 1.804112415015879378E-16 ) ) ;
#2993 = DIRECTION ( 'NONE',  ( 0.000000000000000000, 0.000000000000000000, -1.000000000000000000 ) ) ;
#2994 = CARTESIAN_POINT ( 'NONE',  ( 6.305975611789820690, -62.57522228252229723, -3.271841503593345024 ) ) ;
#2995 = CARTESIAN_POINT ( 'NONE',  ( -6.239404450008960268, -62.05055862403510503, 1.429382062327010150 ) ) ;
#2996 = EDGE_CURVE ( 'NONE', #4883, #6624, #6206, .T. ) ;
#2997 = ADVANCED_FACE ( 'NONE', ( #3323 ), #2752, .T. ) ;
#2998 = VECTOR ( 'NONE', #4419, 1000.000000000000114 ) ;
#2999 = CARTESIAN_POINT ( 'NONE',  ( -5.689067437457130616, -61.48253059702771850, 3.675478928603590489 ) ) ;
#3000 = CARTESIAN_POINT ( 'NONE',  ( -18.14656847176053844, 14.09764149780733966, -2.671436925771696114 ) ) ;
#3001 = DIRECTION ( 'NONE',  ( -0.9492883822130744331, 0.3144066910790611624, 0.000000000000000000 ) ) ;
#3002 = ADVANCED_FACE ( 'NONE', ( #6350 ), #1073, .F. ) ;
#3003 = EDGE_CURVE ( 'NONE', #5506, #1000, #2795, .T. ) ;
#3004 = CARTESIAN_POINT ( 'NONE',  ( 4.061787823018702781, -64.57068682332180742, -1.219517233498399245 ) ) ;
#3005 = VECTOR ( 'NONE', #5774, 999.9999999999998863 ) ;
#3006 = B_SPLINE_SURFACE_WITH_KNOTS ( 'NONE', 1, 3, ( 
 ( #4753, #3543, #5361, #5286 ),
 ( #3608, #2972, #7073, #1910 ) ),
 .UNSPECIFIED., .F., .F., .F.,
 ( 2, 2 ),
 ( 4, 4 ),
 ( 0.000000000000000000, 1.000000000000000000 ),
 ( 0.000000000000000000, 1.000000000000000000 ),
 .UNSPECIFIED. ) ;
#3007 = CARTESIAN_POINT ( 'NONE',  ( 2.906897738665179975, -66.25564029441702019, 0.8681355557765302322 ) ) ;
#3008 = CARTESIAN_POINT ( 'NONE',  ( -35.54168210215661361, 14.82156649444488394, -1.500000000001999956 ) ) ;
#3009 = VERTEX_POINT ( 'NONE', #3926 ) ;
#3010 = CARTESIAN_POINT ( 'NONE',  ( -5.904042796847299712, -62.42803713013675093, 3.506543003539000392 ) ) ;
#3011 = CIRCLE ( 'NONE', #6280, 2.500000000000000444 ) ;
#3012 = DIRECTION ( 'NONE',  ( 0.9999836672264332815, -0.005715354789859975783, 0.000000000000000000 ) ) ;
#3013 = DIRECTION ( 'NONE',  ( 0.8545275983175482093, 0.5194059912184716410, 5.242814362801270410E-16 ) ) ;
#3014 = CARTESIAN_POINT ( 'NONE',  ( -2.392055737067099841, -65.19778216667813808, -1.190937291917544050 ) ) ;
#3015 = CARTESIAN_POINT ( 'NONE',  ( -6.097705871868670080, -61.85866295707492668, 3.539665806518350610 ) ) ;
#3016 = DIRECTION ( 'NONE',  ( 0.9999836672264331705, -0.005715354789859876036, 0.000000000000000000 ) ) ;
#3017 = CLOSED_SHELL ( 'NONE', ( #1082, #6699, #1693 ) ) ;
#3018 = ORIENTED_EDGE ( 'NONE', *, *, #393, .T. ) ;
#3019 = ORIENTED_EDGE ( 'NONE', *, *, #1023, .F. ) ;
#3020 = ORIENTED_EDGE ( 'NONE', *, *, #2374, .T. ) ;
#3021 = CARTESIAN_POINT ( 'NONE',  ( -13.12502771320784056, -36.71825441132875767, 1.026284428608169819 ) ) ;
#3022 = AXIS2_PLACEMENT_3D ( 'NONE', #6723, #856, #3156 ) ;
#3023 = AXIS2_PLACEMENT_3D ( 'NONE', #4223, #3687, #1368 ) ;
#3024 = LINE ( 'NONE', #6433, #5704 ) ;
#3025 = CARTESIAN_POINT ( 'NONE',  ( 3.257640280419950241, -66.06664283717124420, -1.252360977842533751 ) ) ;
#3026 = VECTOR ( 'NONE', #4409, 999.9999999999998863 ) ;
#3027 = DIRECTION ( 'NONE',  ( -5.715354789845005112E-18, -9.999836672264339449E-16, 1.000000000000000000 ) ) ;
#3028 = AXIS2_PLACEMENT_3D ( 'NONE', #5238, #6395, #2917 ) ;
#3029 = EDGE_LOOP ( 'NONE', ( #1715, #2294, #1630, #2805 ) ) ;
#3030 = ORIENTED_EDGE ( 'NONE', *, *, #1540, .T. ) ;
#3031 = VECTOR ( 'NONE', #3674, 1000.000000000000000 ) ;
#3032 =( GEOMETRIC_REPRESENTATION_CONTEXT ( 3 ) GLOBAL_UNCERTAINTY_ASSIGNED_CONTEXT ( ( #5400 ) ) GLOBAL_UNIT_ASSIGNED_CONTEXT ( ( #4209, #7035, #1386 ) ) REPRESENTATION_CONTEXT ( 'NONE', 'WORKASPACE' ) );
#3033 = EDGE_CURVE ( 'NONE', #380, #1005, #511, .T. ) ;
#3034 = CARTESIAN_POINT ( 'NONE',  ( -14.02739156872318027, -37.17434273187110705, -0.4662714048949997969 ) ) ;
#3035 = CIRCLE ( 'NONE', #47, 1.000000000000000444 ) ;
#3036 = FACE_OUTER_BOUND ( 'NONE', #3741, .T. ) ;
#3037 = VECTOR ( 'NONE', #5728, 1000.000000000000000 ) ;
#3038 = FACE_OUTER_BOUND ( 'NONE', #301, .T. ) ;
#3039 = DIRECTION ( 'NONE',  ( 0.000000000000000000, 0.000000000000000000, -1.000000000000000000 ) ) ;
#3040 = DIRECTION ( 'NONE',  ( -0.9999836672264333925, 0.005715354789844381486, 0.000000000000000000 ) ) ;
#3041 = AXIS2_PLACEMENT_3D ( 'NONE', #7340, #1659, #6857 ) ;
#3042 = EDGE_CURVE ( 'NONE', #3635, #3563, #7427, .T. ) ;
#3043 = CARTESIAN_POINT ( 'NONE',  ( 1.397902174090916105, -65.57924198930768966, 0.6644065888002452791 ) ) ;
#3044 = VECTOR ( 'NONE', #201, 1000.000000000000000 ) ;
#3045 = CIRCLE ( 'NONE', #5106, 6.500000000000001776 ) ;
#3046 = CARTESIAN_POINT ( 'NONE',  ( -7.741417275248890562, 12.33509147838778830, 1.214306433183764966E-14 ) ) ;
#3047 = DIRECTION ( 'NONE',  ( 0.000000000000000000, 0.000000000000000000, 1.000000000000000000 ) ) ;
#3048 = CARTESIAN_POINT ( 'NONE',  ( -2.599597233209017144, -55.21935138117550679, -2.163518569292217641 ) ) ;
#3049 = CARTESIAN_POINT ( 'NONE',  ( -6.238986924797109701, -58.62463756020586914, -0.4569988612983747478 ) ) ;
#3050 = ORIENTED_EDGE ( 'NONE', *, *, #5872, .T. ) ;
#3051 = CARTESIAN_POINT ( 'NONE',  ( 26.98506241315388010, -34.62942011279275079, -0.5000000000000346390 ) ) ;
#3052 = EDGE_CURVE ( 'NONE', #6755, #3946, #661, .T. ) ;
#3053 = EDGE_CURVE ( 'NONE', #210, #6757, #3035, .T. ) ;
#3054 = CARTESIAN_POINT ( 'NONE',  ( 14.29543924104632779, -35.83228874779774742, 2.999999999999964473 ) ) ;
#3055 = CARTESIAN_POINT ( 'NONE',  ( 17.88843813672055916, -40.41242482140538073, -4.025211077939830175E-14 ) ) ;
#3056 = UNCERTAINTY_MEASURE_WITH_UNIT (LENGTH_MEASURE( 1.000000000000000082E-05 ), #2434, 'distance_accuracy_value', 'NONE');
#3057 = CARTESIAN_POINT ( 'NONE',  ( 3.331090576803830139, -65.95739139720836874, 0.8111086825117052035 ) ) ;
#3058 = CARTESIAN_POINT ( 'NONE',  ( 1.276103242900551882, -55.15251840166065733, -1.809563881513800876 ) ) ;
#3059 = CARTESIAN_POINT ( 'NONE',  ( 5.267626090836840191, -63.86700364562991439, -1.442031773567929775 ) ) ;
#3060 = FACE_OUTER_BOUND ( 'NONE', #5291, .T. ) ;
#3061 = ORIENTED_EDGE ( 'NONE', *, *, #4996, .F. ) ;
#3062 = ORIENTED_EDGE ( 'NONE', *, *, #2466, .T. ) ;
#3063 = ORIENTED_EDGE ( 'NONE', *, *, #3053, .T. ) ;
#3064 = DIRECTION ( 'NONE',  ( -0.9147661038495488173, 0.4039838799357178822, 1.577721810442023611E-30 ) ) ;
#3065 = CARTESIAN_POINT ( 'NONE',  ( 25.15036705625666258, 26.15624279088186910, 3.000000000000026645 ) ) ;
#3066 = CARTESIAN_POINT ( 'NONE',  ( -5.310432382237169513, -59.25281681403794209, -2.339912608914485936 ) ) ;
#3067 = ORIENTED_EDGE ( 'NONE', *, *, #3686, .T. ) ;
#3068 = ORIENTED_EDGE ( 'NONE', *, *, #2334, .F. ) ;
#3069 = VERTEX_POINT ( 'NONE', #2947 ) ;
#3070 = DIRECTION ( 'NONE',  ( 5.715354789845005112E-18, 9.999836672264339449E-16, -1.000000000000000000 ) ) ;
#3071 = CARTESIAN_POINT ( 'NONE',  ( 19.86817077757007510, -41.71399671145089627, 2.999999999999958256 ) ) ;
#3072 = CARTESIAN_POINT ( 'NONE',  ( 4.747874937083381930, -62.01186481602808698, -2.352241412846060697 ) ) ;
#3073 = CARTESIAN_POINT ( 'NONE',  ( 1.316624512147740012, -66.75104842734066324, 3.019790780136459851 ) ) ;
#3074 = ORIENTED_EDGE ( 'NONE', *, *, #3142, .F. ) ;
#3075 = EDGE_LOOP ( 'NONE', ( #6136, #4863, #6461, #4194 ) ) ;
#3076 =( NAMED_UNIT ( * ) PLANE_ANGLE_UNIT ( ) SI_UNIT ( $, .RADIAN. ) );
#3077 = B_SPLINE_CURVE_WITH_KNOTS ( 'NONE', 3,
 ( #4830, #5893, #7114, #1955 ),
 .UNSPECIFIED., .F., .F.,
 ( 4, 4 ),
 ( 0.000000000000000000, 1.000000000000000000 ),
 .UNSPECIFIED. ) ;
#3078 = CARTESIAN_POINT ( 'NONE',  ( -5.211262431554310126, -59.36811747016641050, -0.7503612693867500738 ) ) ;
#3079 = DIRECTION ( 'NONE',  ( 0.3128416502900970286, -0.9445788350777319931, 0.09950339776592319330 ) ) ;
#3080 = DIRECTION ( 'NONE',  ( 1.000000000000000000, 0.000000000000000000, 0.000000000000000000 ) ) ;
#3081 = CARTESIAN_POINT ( 'NONE',  ( -4.642435027186547103, -56.98634068404612663, -2.320710962605212480 ) ) ;
#3082 = EDGE_CURVE ( 'NONE', #6872, #380, #4135, .T. ) ;
#3083 = ORIENTED_EDGE ( 'NONE', *, *, #3785, .F. ) ;
#3084 = DIRECTION ( 'NONE',  ( 0.3128416502900970286, -0.9445788350777319931, 0.09950339776592319330 ) ) ;
#3085 = CARTESIAN_POINT ( 'NONE',  ( 20.45577244917009097, -23.95683820943714792, -3.000000000000024869 ) ) ;
#3086 = DIRECTION ( 'NONE',  ( 0.000000000000000000, 0.000000000000000000, -1.000000000000000000 ) ) ;
#3087 = CARTESIAN_POINT ( 'NONE',  ( -5.524241737545620090, -57.12730840725460979, 1.694319224817255165 ) ) ;
#3088 = CARTESIAN_POINT ( 'NONE',  ( -6.026198395890769888, -63.94474587426248036, 1.222360836057740041 ) ) ;
#3089 = EDGE_CURVE ( 'NONE', #6662, #5560, #4662, .T. ) ;
#3090 = CARTESIAN_POINT ( 'NONE',  ( -16.56077119915742202, 1.636355435069148490, -2.993845543551538313 ) ) ;
#3091 = EDGE_CURVE ( 'NONE', #5062, #1506, #4248, .T. ) ;
#3092 = ORIENTED_EDGE ( 'NONE', *, *, #3091, .F. ) ;
#3093 = EDGE_LOOP ( 'NONE', ( #1243, #329, #6377, #2483 ) ) ;
#3094 = CARTESIAN_POINT ( 'NONE',  ( -34.88460058024266175, 16.28046363954879183, -0.7438455435519999437 ) ) ;
#3095 = LINE ( 'NONE', #3065, #3633 ) ;
#3096 = CARTESIAN_POINT ( 'NONE',  ( -1.110895189285712181, -65.77251424999820983, -2.870029284013874360 ) ) ;
#3097 = CARTESIAN_POINT ( 'NONE',  ( 1.878435065497310541, -54.43101827334665899, 2.142267462834059888 ) ) ;
#3098 = EDGE_CURVE ( 'NONE', #2020, #2611, #3527, .T. ) ;
#3099 = EDGE_LOOP ( 'NONE', ( #3376, #4204, #962, #5870 ) ) ;
#3100 = VERTEX_POINT ( 'NONE', #14 ) ;
#3101 = ORIENTED_EDGE ( 'NONE', *, *, #1900, .F. ) ;
#3102 = CARTESIAN_POINT ( 'NONE',  ( 9.998427761233271482, -32.39925913208585939, 2.999999999999967581 ) ) ;
#3103 = CARTESIAN_POINT ( 'NONE',  ( -32.92087242456759100, 14.53869105662955796, -2.993845543551514776 ) ) ;
#3104 = DIRECTION ( 'NONE',  ( 0.4039838799357100552, 0.9147661038495522590, 1.399039571475124858E-16 ) ) ;
#3105 = CARTESIAN_POINT ( 'NONE',  ( -6.129265975028279634, -62.42766041111902098, -0.6909925287373350766 ) ) ;
#3106 = ORIENTED_EDGE ( 'NONE', *, *, #303, .F. ) ;
#3107 = EDGE_CURVE ( 'NONE', #1377, #5715, #7249, .T. ) ;
#3108 = VECTOR ( 'NONE', #3461, 1000.000000000000000 ) ;
#3109 = ORIENTED_EDGE ( 'NONE', *, *, #3089, .T. ) ;
#3110 = PLANE ( 'NONE',  #1847 ) ;
#3111 = CARTESIAN_POINT ( 'NONE',  ( 1.275220786007323914, -54.66846601681689322, 0.1350250863793004130 ) ) ;
#3112 = CIRCLE ( 'NONE', #4207, 3.750000000000000444 ) ;
#3113 = DIRECTION ( 'NONE',  ( 0.8688689365825388311, 0.4950421911735690128, -8.411011176753756085E-16 ) ) ;
#3114 = CARTESIAN_POINT ( 'NONE',  ( -6.322565549722802380, -62.54715718787130641, 3.405899984212338971 ) ) ;
#3115 = CARTESIAN_POINT ( 'NONE',  ( -5.789985532050487826, -60.41058001130513588, -0.4326874901607719592 ) ) ;
#3116 = ORIENTED_EDGE ( 'NONE', *, *, #2475, .T. ) ;
#3117 = CARTESIAN_POINT ( 'NONE',  ( -14.41480805056212056, -36.00459628421619840, -4.334038357861370372 ) ) ;
#3118 = EDGE_CURVE ( 'NONE', #321, #3534, #2193, .T. ) ;
#3119 = DIRECTION ( 'NONE',  ( 5.715354789845004342E-18, 9.999836672264337477E-16, -1.000000000000000000 ) ) ;
#3120 = CIRCLE ( 'NONE', #7337, 11.50000000000000178 ) ;
#3121 = CARTESIAN_POINT ( 'NONE',  ( 20.29543457672885154, -41.45429371584162226, 2.999999999999958700 ) ) ;
#3122 = LINE ( 'NONE', #3237, #755 ) ;
#3123 = CARTESIAN_POINT ( 'NONE',  ( -5.895051854024569771, -62.45358532148892294, 3.505907163650189950 ) ) ;
#3124 = CARTESIAN_POINT ( 'NONE',  ( -2.038541806680159940, -53.77797276486428046, -0.2805255711276150588 ) ) ;
#3125 = CARTESIAN_POINT ( 'NONE',  ( 15.08188723176695056, -33.99092340910145538, 5.072392329257909616 ) ) ;
#3126 = ORIENTED_EDGE ( 'NONE', *, *, #6164, .T. ) ;
#3127 = ORIENTED_EDGE ( 'NONE', *, *, #4764, .T. ) ;
#3128 = AXIS2_PLACEMENT_3D ( 'NONE', #318, #7233, #2576 ) ;
#3129 = PRODUCT_DEFINITION_SHAPE ( 'NONE', 'NONE',  #4117 ) ;
#3130 = ADVANCED_FACE ( 'NONE', ( #6316 ), #3439, .F. ) ;
#3131 = LINE ( 'NONE', #2580, #6533 ) ;
#3132 = CARTESIAN_POINT ( 'NONE',  ( 1.597826897138040048, -55.24069855439622501, 0.3109211183784004184 ) ) ;
#3133 = CLOSED_SHELL ( 'NONE', ( #3605, #2097, #2919, #1670, #3189, #4897, #6788, #6935, #5411, #2997, #3572, #6105 ) ) ;
#3134 = CARTESIAN_POINT ( 'NONE',  ( -5.977281909777053315, -62.42932436707042854, 1.407931773894181227 ) ) ;
#3135 = ORIENTED_EDGE ( 'NONE', *, *, #2818, .T. ) ;
#3136 = ORIENTED_EDGE ( 'NONE', *, *, #3774, .T. ) ;
#3137 = ORIENTED_EDGE ( 'NONE', *, *, #235, .F. ) ;
#3138 = CIRCLE ( 'NONE', #5082, 1.000000000000000000 ) ;
#3139 = CIRCLE ( 'NONE', #6878, 0.7499999999999872324 ) ;
#3140 = ADVANCED_FACE ( 'NONE', ( #5113 ), #6654, .T. ) ;
#3141 = SHAPE_DEFINITION_REPRESENTATION ( #5433, #4460 ) ;
#3142 = EDGE_CURVE ( 'NONE', #1377, #5998, #1754, .T. ) ;
#3143 = DIRECTION ( 'NONE',  ( 0.8039121061460955397, -0.3550279469270867794, 0.4771587602596085165 ) ) ;
#3144 = DIRECTION ( 'NONE',  ( -5.715354789845005112E-18, -9.999836672264339449E-16, 1.000000000000000000 ) ) ;
#3145 = DIRECTION ( 'NONE',  ( -0.2023178344681530183, 0.9793199139485100346, 8.673617379884158732E-16 ) ) ;
#3146 = CARTESIAN_POINT ( 'NONE',  ( 5.854317997614909785, -64.22630450538810010, 2.635376777014039718 ) ) ;
#3147 = ORIENTED_EDGE ( 'NONE', *, *, #404, .T. ) ;
#3148 = AXIS2_PLACEMENT_3D ( 'NONE', #6803, #5038, #5076 ) ;
#3149 = AXIS2_PLACEMENT_3D ( 'NONE', #6663, #5478, #305 ) ;
#3150 = SHAPE_REPRESENTATION ( 'Pliers Left Handle Arm', ( #751 ), #3032 ) ;
#3151 = CARTESIAN_POINT ( 'NONE',  ( -9.311346830843410416, -51.41373841511902043, 2.533728595105000370 ) ) ;
#3152 = AXIS2_PLACEMENT_3D ( 'NONE', #3559, #2581, #4845 ) ;
#3153 = CARTESIAN_POINT ( 'NONE',  ( -3.222464925939095171, -55.48519077065235194, -0.1302151132178846482 ) ) ;
#3154 = VECTOR ( 'NONE', #6692, 1000.000000000000000 ) ;
#3155 = EDGE_LOOP ( 'NONE', ( #5748, #6128, #5756, #5965, #4199, #2111 ) ) ;
#3156 = DIRECTION ( 'NONE',  ( 5.715354789845005112E-18, 9.999836672264339449E-16, -1.000000000000000000 ) ) ;
#3157 = VECTOR ( 'NONE', #3104, 1000.000000000000000 ) ;
#3158 = DIRECTION ( 'NONE',  ( -1.602374898470634869E-16, 1.442524254523139935E-17, 1.000000000000000000 ) ) ;
#3159 = CARTESIAN_POINT ( 'NONE',  ( -2.726528979675269859, -65.60628988660214134, -2.897654743900204721 ) ) ;
#3160 = AXIS2_PLACEMENT_3D ( 'NONE', #6265, #6342, #52 ) ;
#3161 = ORIENTED_EDGE ( 'NONE', *, *, #2605, .T. ) ;
#3162 = AXIS2_PLACEMENT_3D ( 'NONE', #3505, #4155, #3577 ) ;
#3163 = CARTESIAN_POINT ( 'NONE',  ( 27.98760434640042050, 26.43260972569849443, -1.493845543551990174 ) ) ;
#3164 = DIRECTION ( 'NONE',  ( -0.9828140593167951078, 0.1845982795403117438, 1.789781334969680744E-16 ) ) ;
#3165 = CYLINDRICAL_SURFACE ( 'NONE', #3276, 0.9999999999999998890 ) ;
#3166 = CARTESIAN_POINT ( 'NONE',  ( 5.267626090836840191, -63.86700364562991439, -1.442031773567929775 ) ) ;
#3167 = DIRECTION ( 'NONE',  ( 0.6513146796332659472, 0.5900073775824578037, -0.4771587602596093491 ) ) ;
#3168 = CARTESIAN_POINT ( 'NONE',  ( 1.455885123031280148, -67.63619251397972221, 2.328451870335179752 ) ) ;
#3169 = CYLINDRICAL_SURFACE ( 'NONE', #1698, 1.000000000000000888 ) ;
#3170 = ORIENTED_EDGE ( 'NONE', *, *, #2455, .T. ) ;
#3171 = VERTEX_POINT ( 'NONE', #1227 ) ;
#3172 = VERTEX_POINT ( 'NONE', #616 ) ;
#3173 = DIRECTION ( 'NONE',  ( 0.000000000000000000, 0.000000000000000000, 1.000000000000000000 ) ) ;
#3174 = LINE ( 'NONE', #3210, #6890 ) ;
#3175 = CARTESIAN_POINT ( 'NONE',  ( -3.096824821213254975, -64.92072129780139278, 1.460348123614904514 ) ) ;
#3176 = DIRECTION ( 'NONE',  ( 0.9999836672264332815, -0.005715354789845002517, 0.000000000000000000 ) ) ;
#3177 = CARTESIAN_POINT ( 'NONE',  ( -3.758252532389416256, -55.38071557709576354, 1.827664687072033889 ) ) ;
#3178 = ORIENTED_EDGE ( 'NONE', *, *, #6154, .T. ) ;
#3179 = VERTEX_POINT ( 'NONE', #2904 ) ;
#3180 = EDGE_CURVE ( 'NONE', #2064, #7211, #7015, .T. ) ;
#3181 = EDGE_LOOP ( 'NONE', ( #5071, #311, #5954, #5446, #3068, #5989 ) ) ;
#3182 = ORIENTED_EDGE ( 'NONE', *, *, #668, .T. ) ;
#3183 = LINE ( 'NONE', #6215, #3522 ) ;
#3184 = DIRECTION ( 'NONE',  ( -0.9147661038495521479, 0.4039838799357104993, 5.097713713877666172E-16 ) ) ;
#3185 = CARTESIAN_POINT ( 'NONE',  ( 15.26844188666829893, -16.88471001685938333, -1.691355389077386917E-14 ) ) ;
#3186 = CARTESIAN_POINT ( 'NONE',  ( -2.887726905928315269, -66.20272978495717098, -0.9560320787877147897 ) ) ;
#3187 = ORIENTED_EDGE ( 'NONE', *, *, #2697, .T. ) ;
#3188 = EDGE_CURVE ( 'NONE', #2830, #7250, #2237, .T. ) ;
#3189 = ADVANCED_FACE ( 'NONE', ( #2416, #7016 ), #4692, .T. ) ;
#3190 = CARTESIAN_POINT ( 'NONE',  ( 27.65533861039811114, -36.12687000486613442, -3.599551212651874721E-14 ) ) ;
#3191 = CARTESIAN_POINT ( 'NONE',  ( -5.996378862946620814, -62.15612413928192836, 3.522786485084270058 ) ) ;
#3192 = ORIENTED_EDGE ( 'NONE', *, *, #2406, .T. ) ;
#3193 = DIRECTION ( 'NONE',  ( -0.08966155106958693943, -0.9959722919136836383, 0.000000000000000000 ) ) ;
#3194 = CARTESIAN_POINT ( 'NONE',  ( -105.7473861751082040, -118.0666774205683822, 2.999999999999881428 ) ) ;
#3195 = SHAPE_REPRESENTATION ( 'MAS-689', ( #6182, #1007, #6305, #3404, #5586, #4494, #997 ), #7012 ) ;
#3196 = EDGE_CURVE ( 'NONE', #3216, #3712, #826, .T. ) ;
#3197 = ORIENTED_EDGE ( 'NONE', *, *, #2894, .T. ) ;
#3198 = FACE_OUTER_BOUND ( 'NONE', #3269, .T. ) ;
#3199 = FACE_OUTER_BOUND ( 'NONE', #735, .T. ) ;
#3200 = DIRECTION ( 'NONE',  ( -0.4950421911735689018, 0.8688689365825386091, 0.000000000000000000 ) ) ;
#3201 = PRODUCT_DEFINITION_CONTEXT ( 'detailed design', #3691, 'design' ) ;
#3202 = CARTESIAN_POINT ( 'NONE',  ( -8.408982975328068932, -50.95765009457664974, 2.526284428608170263 ) ) ;
#3203 = CARTESIAN_POINT ( 'NONE',  ( 14.29543924104632779, -35.83228874779774742, 2.999999999999964473 ) ) ;
#3204 = CARTESIAN_POINT ( 'NONE',  ( 5.693513582185560473, -64.15546253253084785, -1.561391656022143914 ) ) ;
#3205 = DIRECTION ( 'NONE',  ( 0.3536350175650656014, 0.3203478684871221560, 0.8788171126619651607 ) ) ;
#3206 = ORIENTED_EDGE ( 'NONE', *, *, #5925, .T. ) ;
#3207 = DIRECTION ( 'NONE',  ( 0.9999836672264335036, -0.005715354789845008589, 0.000000000000000000 ) ) ;
#3208 = ORIENTED_EDGE ( 'NONE', *, *, #4353, .F. ) ;
#3209 = CARTESIAN_POINT ( 'NONE',  ( -14.63584665781298000, 13.71482652663877566, 1.357730697108428863 ) ) ;
#3210 = CARTESIAN_POINT ( 'NONE',  ( 24.99346688245966419, 26.01411140189437177, 0.006154456448490951831 ) ) ;
#3211 = CARTESIAN_POINT ( 'NONE',  ( 1.985288149635364929, -66.63130641047898450, -3.284835754603986580 ) ) ;
#3212 = DIRECTION ( 'NONE',  ( -5.715354789845005112E-18, -9.999836672264339449E-16, 1.000000000000000000 ) ) ;
#3213 = CARTESIAN_POINT ( 'NONE',  ( -1.036475255397104833, -54.28545530925913454, 1.984742741622252948 ) ) ;
#3214 = ORIENTED_EDGE ( 'NONE', *, *, #4171, .F. ) ;
#3215 = ORIENTED_EDGE ( 'NONE', *, *, #4072, .T. ) ;
#3216 = VERTEX_POINT ( 'NONE', #689 ) ;
#3217 = PRODUCT_CONTEXT ( 'NONE', #5258, 'mechanical' ) ;
#3218 = DIRECTION ( 'NONE',  ( 2.207673464680433438E-16, -2.241093068000311301E-16, 1.000000000000000000 ) ) ;
#3219 = EDGE_CURVE ( 'NONE', #181, #4378, #3761, .T. ) ;
#3220 = DIRECTION ( 'NONE',  ( 0.3128463504745289669, 0.9445772445362837777, 0.09950371902099817978 ) ) ;
#3221 = DIRECTION ( 'NONE',  ( 0.4950421911735688463, -0.8688689365825387201, -8.660254037844397269E-16 ) ) ;
#3222 = CARTESIAN_POINT ( 'NONE',  ( 3.949972843796054178, -66.18831294452250802, -1.427832076542613793 ) ) ;
#3223 = ORIENTED_EDGE ( 'NONE', *, *, #2455, .F. ) ;
#3224 = VERTEX_POINT ( 'NONE', #1858 ) ;
#3225 = ORIENTED_EDGE ( 'NONE', *, *, #3142, .T. ) ;
#3226 = CYLINDRICAL_SURFACE ( 'NONE', #1472, 3.299999999999999378 ) ;
#3227 = CARTESIAN_POINT ( 'NONE',  ( 2.986904076224405014, -66.15109244657664078, 2.931604786918900363 ) ) ;
#3228 = CIRCLE ( 'NONE', #4200, 5.000000000000000000 ) ;
#3229 = DIRECTION ( 'NONE',  ( 0.9999836672264332815, -0.005715354789859975783, 0.000000000000000000 ) ) ;
#3230 = LINE ( 'NONE', #2062, #5788 ) ;
#3231 = PRODUCT_RELATED_PRODUCT_CATEGORY ( 'part', '', ( #255 ) ) ;
#3232 = EDGE_LOOP ( 'NONE', ( #2137, #773, #801, #4318, #3590, #5094 ) ) ;
#3233 = CIRCLE ( 'NONE', #4011, 1.000000000000001776 ) ;
#3234 = EDGE_CURVE ( 'NONE', #6135, #5520, #1820, .T. ) ;
#3235 = CARTESIAN_POINT ( 'NONE',  ( -14.70408710852078116, -35.66654345889202204, -3.000000000000036415 ) ) ;
#3236 = ADVANCED_FACE ( 'NONE', ( #4225 ), #202, .T. ) ;
#3237 = CARTESIAN_POINT ( 'NONE',  ( 26.82878048574519525, 24.30342645899339615, 3.000000000000024425 ) ) ;
#3238 = CYLINDRICAL_SURFACE ( 'NONE', #488, 20.00000000000000000 ) ;
#3239 = PLANE ( 'NONE',  #3651 ) ;
#3240 = VECTOR ( 'NONE', #4413, 1000.000000000000000 ) ;
#3241 = CARTESIAN_POINT ( 'NONE',  ( -3.551508372363994859, -54.02225908916108210, 1.181396430060940306 ) ) ;
#3242 = DIRECTION ( 'NONE',  ( 0.3128463504745285229, 0.9445772445362839997, 0.09950371902099811039 ) ) ;
#3243 = ORIENTED_EDGE ( 'NONE', *, *, #162, .T. ) ;
#3244 = ORIENTED_EDGE ( 'NONE', *, *, #7010, .T. ) ;
#3245 = AXIS2_PLACEMENT_3D ( 'NONE', #4730, #2356, #6917 ) ;
#3246 = PLANE ( 'NONE',  #6166 ) ;
#3247 = PLANE ( 'NONE',  #148 ) ;
#3248 = CARTESIAN_POINT ( 'NONE',  ( 4.964513617332250384, -59.39532806039484569, 1.236961020452715054 ) ) ;
#3249 = CARTESIAN_POINT ( 'NONE',  ( -9.358272925367041140, -51.27205205187813419, 2.526284428608170263 ) ) ;
#3250 = CARTESIAN_POINT ( 'NONE',  ( -6.177096350592991669, -59.51804186297885479, 1.565423707298817080 ) ) ;
#3251 = ORIENTED_EDGE ( 'NONE', *, *, #2818, .F. ) ;
#3252 = ORIENTED_EDGE ( 'NONE', *, *, #5690, .F. ) ;
#3253 = ORIENTED_EDGE ( 'NONE', *, *, #4124, .F. ) ;
#3254 = DIRECTION ( 'NONE',  ( 1.000000000000000000, 0.000000000000000000, 0.000000000000000000 ) ) ;
#3255 = CARTESIAN_POINT ( 'NONE',  ( 14.29543924104632779, -35.83228874779774742, -3.556183125752454544E-14 ) ) ;
#3256 = PLANE ( 'NONE',  #5706 ) ;
#3257 = LINE ( 'NONE', #2125, #6078 ) ;
#3258 = CARTESIAN_POINT ( 'NONE',  ( 5.904685685680689744, -64.36828453093134783, 1.045689304822035037 ) ) ;
#3259 = EDGE_LOOP ( 'NONE', ( #1215, #624 ) ) ;
#3260 = AXIS2_PLACEMENT_3D ( 'NONE', #7207, #2117, #998 ) ;
#3261 = PLANE ( 'NONE',  #7236 ) ;
#3262 = CARTESIAN_POINT ( 'NONE',  ( 16.88097023408849751, 15.29198909576265919, 0.4060579846640053336 ) ) ;
#3263 = CARTESIAN_POINT ( 'NONE',  ( -5.524241737545620090, -57.12730840725460979, 1.694319224817255165 ) ) ;
#3264 = AXIS2_PLACEMENT_3D ( 'NONE', #1323, #5969, #2449 ) ;
#3265 = AXIS2_PLACEMENT_3D ( 'NONE', #1075, #2197, #1194 ) ;
#3266 = DIRECTION ( 'NONE',  ( -0.9999836672264333925, 0.005715354789844381486, 0.000000000000000000 ) ) ;
#3267 = DIRECTION ( 'NONE',  ( -5.715354789860003484E-18, -9.999836672264337477E-16, 1.000000000000000000 ) ) ;
#3268 = VECTOR ( 'NONE', #3027, 1000.000000000000000 ) ;
#3269 = EDGE_LOOP ( 'NONE', ( #6616, #6172, #4347, #7146 ) ) ;
#3270 = ORIENTED_EDGE ( 'NONE', *, *, #3335, .T. ) ;
#3271 = EDGE_CURVE ( 'NONE', #2474, #4883, #4118, .T. ) ;
#3272 = CIRCLE ( 'NONE', #4128, 5.000000000000000000 ) ;
#3273 = CIRCLE ( 'NONE', #4616, 147.0000000000000284 ) ;
#3274 = LINE ( 'NONE', #2026, #5211 ) ;
#3275 = CARTESIAN_POINT ( 'NONE',  ( 10.46182022341160867, 4.774967812772741738, 3.000000000000004885 ) ) ;
#3276 = AXIS2_PLACEMENT_3D ( 'NONE', #5490, #2603, #4913 ) ;
#3277 = DIRECTION ( 'NONE',  ( -5.715354789845005112E-18, -9.999836672264339449E-16, 1.000000000000000000 ) ) ;
#3278 = VECTOR ( 'NONE', #7310, 1000.000000000000114 ) ;
#3279 = CARTESIAN_POINT ( 'NONE',  ( 2.066956868921485224, -53.66058936408188629, 0.4281972772843347652 ) ) ;
#3280 = CARTESIAN_POINT ( 'NONE',  ( -4.860610968486169803, -1.172374092613760022, -17.67054229618195293 ) ) ;
#3281 = AXIS2_PLACEMENT_3D ( 'NONE', #1454, #2623, #4932 ) ;
#3282 = ORIENTED_EDGE ( 'NONE', *, *, #6986, .F. ) ;
#3283 = ADVANCED_FACE ( 'NONE', ( #93 ), #6522, .F. ) ;
#3284 = ADVANCED_FACE ( 'NONE', ( #1917 ), #2386, .T. ) ;
#3285 = CYLINDRICAL_SURFACE ( 'NONE', #4831, 140.0000000000000000 ) ;
#3286 = CARTESIAN_POINT ( 'NONE',  ( -12.68712931281627476, 13.22355527668857356, 1.301042606982605321E-14 ) ) ;
#3287 = AXIS2_PLACEMENT_3D ( 'NONE', #2349, #1852, #610 ) ;
#3288 = PLANE ( 'NONE',  #4492 ) ;
#3289 = CARTESIAN_POINT ( 'NONE',  ( -4.559578989909869762, -57.69789612496867903, 1.459412177499654462 ) ) ;
#3290 = CARTESIAN_POINT ( 'NONE',  ( -12.10129460565897475, -12.45149060151658027, -3.000000000000013323 ) ) ;
#3291 = CARTESIAN_POINT ( 'NONE',  ( 35.76131148831677109, 4.835142255982176174, -2.999999999999995559 ) ) ;
#3292 = CARTESIAN_POINT ( 'NONE',  ( -5.253023064401910247, -61.29850624113154822, 1.730934016304810363 ) ) ;
#3293 = EDGE_CURVE ( 'NONE', #815, #7266, #6073, .T. ) ;
#3294 = VECTOR ( 'NONE', #2773, 1000.000000000000000 ) ;
#3295 = EDGE_LOOP ( 'NONE', ( #6436, #6920, #5073 ) ) ;
#3296 = ORIENTED_EDGE ( 'NONE', *, *, #3377, .F. ) ;
#3297 = CARTESIAN_POINT ( 'NONE',  ( 0.000000000000000000, 0.000000000000000000, 0.000000000000000000 ) ) ;
#3299 = FACE_OUTER_BOUND ( 'NONE', #6107, .T. ) ;
#3298 = B_SPLINE_CURVE_WITH_KNOTS ( 'NONE', 3,
 ( #285, #3209, #3809, #2613 ),
 .UNSPECIFIED., .F., .F.,
 ( 4, 4 ),
 ( 0.000000000000000000, 1.000000000000000000 ),
 .UNSPECIFIED. ) ;
#3300 = DIRECTION ( 'NONE',  ( 0.000000000000000000, 0.000000000000000000, 1.000000000000000000 ) ) ;
#3301 = DIRECTION ( 'NONE',  ( -0.08966155106958693943, -0.9959722919136836383, 0.000000000000000000 ) ) ;
#3302 = SPHERICAL_SURFACE ( 'NONE', #6886, 7.844444444444450326 ) ;
#3303 = CARTESIAN_POINT ( 'NONE',  ( 6.144163068047750365, -64.45449589790229084, 2.063594979539779661 ) ) ;
#3304 = ORIENTED_EDGE ( 'NONE', *, *, #4816, .F. ) ;
#3305 = CARTESIAN_POINT ( 'NONE',  ( -19.94212619460463287, -40.63668738334721553, -4.075000000000002200E-14 ) ) ;
#3306 = CARTESIAN_POINT ( 'NONE',  ( 7.529070345495034289, 16.11642554373086256, 1.604619215278546562E-14 ) ) ;
#3307 = PLANE ( 'NONE',  #2555 ) ;
#3308 = CARTESIAN_POINT ( 'NONE',  ( 8.409045811045761099, -50.95764513735950629, -2.495037190209991707 ) ) ;
#3309 = DIRECTION ( 'NONE',  ( 0.2223191033124284066, 0.6712482523644728305, 0.7071067811865467956 ) ) ;
#3310 = ORIENTED_EDGE ( 'NONE', *, *, #6150, .F. ) ;
#3311 = ORIENTED_EDGE ( 'NONE', *, *, #2546, .T. ) ;
#3312 = APPLICATION_CONTEXT ( 'automotive_design' ) ;
#3313 = DIRECTION ( 'NONE',  ( 0.9999836672264332815, -0.005715354789860036498, 0.000000000000000000 ) ) ;
#3314 = CARTESIAN_POINT ( 'NONE',  ( -4.763494996734372933, -62.01236420069433564, 2.093068328189249261 ) ) ;
#3315 = ADVANCED_FACE ( 'NONE', ( #913 ), #5596, .T. ) ;
#3316 = DIRECTION ( 'NONE',  ( 0.9999836672264333925, -0.005715354789844960016, 0.000000000000000000 ) ) ;
#3317 = CARTESIAN_POINT ( 'NONE',  ( 3.193531232915834739, -66.77446787883670254, 1.223174286645849929 ) ) ;
#3318 = CARTESIAN_POINT ( 'NONE',  ( 26.67188031194815068, 24.16129507000589527, -2.993845543551515664 ) ) ;
#3319 = ORIENTED_EDGE ( 'NONE', *, *, #3033, .T. ) ;
#3320 = CARTESIAN_POINT ( 'NONE',  ( 14.29543924104632779, -35.83228874779774742, -3.556183125752454544E-14 ) ) ;
#3321 = CARTESIAN_POINT ( 'NONE',  ( -4.816289696271150333, -61.50450503696147564, 2.285640538916479780 ) ) ;
#3322 = LINE ( 'NONE', #5066, #512 ) ;
#3323 = FACE_OUTER_BOUND ( 'NONE', #5725, .T. ) ;
#3324 = EDGE_CURVE ( 'NONE', #1468, #3587, #3122, .T. ) ;
#3325 = EDGE_CURVE ( 'NONE', #6210, #4023, #6157, .T. ) ;
#3326 = CARTESIAN_POINT ( 'NONE',  ( -2.603817572988885054, -64.79915130424556935, -0.08835382460255962467 ) ) ;
#3327 = CARTESIAN_POINT ( 'NONE',  ( 18.06432739836605350, -39.71205113188411673, -0.1321155921049125825 ) ) ;
#3328 = FACE_OUTER_BOUND ( 'NONE', #3791, .T. ) ;
#3329 = ORIENTED_EDGE ( 'NONE', *, *, #3003, .T. ) ;
#3330 = ORIENTED_EDGE ( 'NONE', *, *, #1118, .T. ) ;
#3331 = VERTEX_POINT ( 'NONE', #2677 ) ;
#3332 = DIRECTION ( 'NONE',  ( -5.715354789860003484E-18, -9.999836672264337477E-16, 1.000000000000000000 ) ) ;
#3333 = VERTEX_POINT ( 'NONE', #2106 ) ;
#3334 = DIRECTION ( 'NONE',  ( -0.4950421911735689018, 0.8688689365825386091, 0.000000000000000000 ) ) ;
#3335 = EDGE_CURVE ( 'NONE', #3646, #5827, #4418, .T. ) ;
#3336 = EDGE_CURVE ( 'NONE', #1231, #6822, #4974, .T. ) ;
#3337 = CARTESIAN_POINT ( 'NONE',  ( -41.31559769795914150, -94.79889909491285493, -3.001000000000096257 ) ) ;
#3338 = FACE_OUTER_BOUND ( 'NONE', #918, .T. ) ;
#3339 = CARTESIAN_POINT ( 'NONE',  ( 7.003919171491410189, -62.62977488282763261, 1.976316849587809843 ) ) ;
#3340 = VERTEX_POINT ( 'NONE', #1474 ) ;
#3341 = VERTEX_POINT ( 'NONE', #4453 ) ;
#3342 = ORIENTED_EDGE ( 'NONE', *, *, #5235, .F. ) ;
#3343 = CARTESIAN_POINT ( 'NONE',  ( 18.47982041150265431, -39.47532202006953383, -3.946495907847236140E-14 ) ) ;
#3344 = DIRECTION ( 'NONE',  ( -5.715354789860003484E-18, -9.999836672264337477E-16, 1.000000000000000000 ) ) ;
#3345 = CARTESIAN_POINT ( 'NONE',  ( -2.887726905928315269, -66.20272978495717098, -0.9560320787877147897 ) ) ;
#3346 = EDGE_CURVE ( 'NONE', #1826, #5376, #982, .T. ) ;
#3347 = LINE ( 'NONE', #5739, #3294 ) ;
#3348 = FACE_OUTER_BOUND ( 'NONE', #2631, .T. ) ;
#3349 = CARTESIAN_POINT ( 'NONE',  ( -6.644288653247606646, -62.64468192876543640, 2.431384972305744796 ) ) ;
#3350 = ORIENTED_EDGE ( 'NONE', *, *, #491, .F. ) ;
#3351 = FACE_OUTER_BOUND ( 'NONE', #6500, .T. ) ;
#3352 = CYLINDRICAL_SURFACE ( 'NONE', #2202, 1.000000000000000888 ) ;
#3353 = DIRECTION ( 'NONE',  ( -5.715354789845005112E-18, -9.999836672264339449E-16, 1.000000000000000000 ) ) ;
#3354 = CARTESIAN_POINT ( 'NONE',  ( 6.443572816261259995, -63.55558822192794111, -2.176462561484786118 ) ) ;
#3355 = DIRECTION ( 'NONE',  ( 0.9999836672264331705, -0.005715354789860001804, 0.000000000000000000 ) ) ;
#3356 = AXIS2_PLACEMENT_3D ( 'NONE', #1511, #6703, #3796 ) ;
#3357 = VERTEX_POINT ( 'NONE', #3275 ) ;
#3358 = ORIENTED_EDGE ( 'NONE', *, *, #6202, .F. ) ;
#3359 = ORIENTED_CLOSED_SHELL ( 'NONE', *, #5200, .F. );
#3360 = CARTESIAN_POINT ( 'NONE',  ( -4.847093383240289377, -61.94486680083809205, -1.943810276119404046 ) ) ;
#3361 = DIRECTION ( 'NONE',  ( -0.9147661038495522590, 0.4039838799357101107, 0.000000000000000000 ) ) ;
#3362 = CARTESIAN_POINT ( 'NONE',  ( -15.00216760413269945, 6.625337177075938833, -3.299999999999993161 ) ) ;
#3363 = CARTESIAN_POINT ( 'NONE',  ( -1.308638315835680022, -65.34704488060808103, -0.1780822347184347620 ) ) ;
#3364 = DIRECTION ( 'NONE',  ( 0.6713653717953950162, -0.7411265327553933080, -3.821372782371131388E-16 ) ) ;
#3365 = CARTESIAN_POINT ( 'NONE',  ( -5.870834073365089445, -58.01445613662527734, -0.4538462669607478683 ) ) ;
#3366 = ORIENTED_EDGE ( 'NONE', *, *, #5917, .F. ) ;
#3367 = ORIENTED_EDGE ( 'NONE', *, *, #1780, .F. ) ;
#3368 = VERTEX_POINT ( 'NONE', #3877 ) ;
#3369 = AXIS2_PLACEMENT_3D ( 'NONE', #5142, #607, #6905 ) ;
#3370 = CARTESIAN_POINT ( 'NONE',  ( 24.99346688245966419, 26.01411140189437532, -2.993845543551503674 ) ) ;
#3371 = DIRECTION ( 'NONE',  ( 5.715354789845005112E-18, 9.999836672264339449E-16, -1.000000000000000000 ) ) ;
#3372 = DIRECTION ( 'NONE',  ( -5.715354789845005112E-18, -9.999836672264339449E-16, 1.000000000000000000 ) ) ;
#3373 = AXIS2_PLACEMENT_3D ( 'NONE', #585, #2950, #5265 ) ;
#3374 = CARTESIAN_POINT ( 'NONE',  ( 27.30483170388682623, -34.44723004512029974, -3.426145681764390930E-14 ) ) ;
#3375 = CARTESIAN_POINT ( 'NONE',  ( -2.273841640848679901, -67.16083533941571204, 1.488471302465715018 ) ) ;
#3376 = ORIENTED_EDGE ( 'NONE', *, *, #1392, .F. ) ;
#3377 = EDGE_CURVE ( 'NONE', #7172, #3587, #3837, .T. ) ;
#3378 = CARTESIAN_POINT ( 'NONE',  ( 5.695730293278450596, -62.33055481056936742, -2.502481404895003259 ) ) ;
#3379 = ADVANCED_FACE ( 'NONE', ( #3802 ), #2070, .F. ) ;
#3380 = DIRECTION ( 'NONE',  ( 0.9999836672264332815, -0.005715354789859183882, 0.000000000000000000 ) ) ;
#3381 = LINE ( 'NONE', #6400, #4728 ) ;
#3382 = CARTESIAN_POINT ( 'NONE',  ( 22.42915535073480982, 21.39736943723329432, -1.493845543551513444 ) ) ;
#3383 = CARTESIAN_POINT ( 'NONE',  ( -14.70408710852078116, -35.66654345889202204, -3.000000000000036415 ) ) ;
#3384 = FILL_AREA_STYLE ('',( #43 ) ) ;
#3385 = VERTEX_POINT ( 'NONE', #5555 ) ;
#3386 = ORIENTED_EDGE ( 'NONE', *, *, #542, .T. ) ;
#3387 = EDGE_CURVE ( 'NONE', #6745, #3216, #6899, .T. ) ;
#3388 = AXIS2_PLACEMENT_3D ( 'NONE', #818, #3113, #3334 ) ;
#3389 = CIRCLE ( 'NONE', #1932, 3.750000000000000000 ) ;
#3390 = CARTESIAN_POINT ( 'NONE',  ( 26.87807528571524074, -34.69037653529182563, 2.999999999999965361 ) ) ;
#3391 = CARTESIAN_POINT ( 'NONE',  ( 0.000000000000000000, 0.000000000000000000, -17.67054229618195293 ) ) ;
#3392 = DIRECTION ( 'NONE',  ( -5.715354789860003484E-18, -9.999836672264337477E-16, 1.000000000000000000 ) ) ;
#3393 = CARTESIAN_POINT ( 'NONE',  ( -5.951685856498870386, -64.29772444222471961, -2.487703520802049262 ) ) ;
#3394 = DIRECTION ( 'NONE',  ( 0.4039838799357109433, 0.9147661038495520369, 9.170600743851225078E-16 ) ) ;
#3395 = AXIS2_PLACEMENT_3D ( 'NONE', #7381, #2857, #5777 ) ;
#3396 = VECTOR ( 'NONE', #5133, 1000.000000000000114 ) ;
#3397 = ORIENTED_EDGE ( 'NONE', *, *, #4416, .T. ) ;
#3398 = CARTESIAN_POINT ( 'NONE',  ( 18.63335487545880653, -39.96655599946684845, 3.999999999999960032 ) ) ;
#3399 = CARTESIAN_POINT ( 'NONE',  ( -20.89962323070193406, -41.21687045383659154, -4.133564602976221858E-14 ) ) ;
#3400 = CIRCLE ( 'NONE', #6765, 0.4999999999999918954 ) ;
#3401 = VECTOR ( 'NONE', #6029, 1000.000000000000000 ) ;
#3402 = DIRECTION ( 'NONE',  ( 5.715354789845005112E-18, 9.999836672264339449E-16, -1.000000000000000000 ) ) ;
#3403 = CARTESIAN_POINT ( 'NONE',  ( -2.607408651135029842, -55.80429912246091106, 1.635486251833709881 ) ) ;
#3404 = AXIS2_PLACEMENT_3D ( 'NONE', #1567, #1009, #5463 ) ;
#3405 = VECTOR ( 'NONE', #7143, 1000.000000000000000 ) ;
#3406 = CARTESIAN_POINT ( 'NONE',  ( 18.31184849395311787, -40.14648560017523238, 2.999999999999960032 ) ) ;
#3407 = DIRECTION ( 'NONE',  ( -0.9721221936972339606, -0.2344748185227520099, 0.000000000000000000 ) ) ;
#3408 = AXIS2_PLACEMENT_3D ( 'NONE', #1402, #3086, #5370 ) ;
#3409 = VERTEX_POINT ( 'NONE', #4305 ) ;
#3410 = ORIENTED_EDGE ( 'NONE', *, *, #609, .T. ) ;
#3411 = CIRCLE ( 'NONE', #168, 6.500000000000001776 ) ;
#3412 = VECTOR ( 'NONE', #6361, 1000.000000000000000 ) ;
#3413 = DIRECTION ( 'NONE',  ( 0.2223157560262047083, -0.6712493609847988152, 0.7071067811865449082 ) ) ;
#3414 = ORIENTED_EDGE ( 'NONE', *, *, #827, .F. ) ;
#3415 = LINE ( 'NONE', #6838, #1356 ) ;
#3416 = FACE_OUTER_BOUND ( 'NONE', #1398, .T. ) ;
#3417 = CARTESIAN_POINT ( 'NONE',  ( -9.326988862351289100, -51.36650962737204651, 1.531247206272719374 ) ) ;
#3418 = CARTESIAN_POINT ( 'NONE',  ( 1.894024985814124928, -67.53311321014548696, 0.2080693458549401353 ) ) ;
#3419 = ADVANCED_FACE ( 'NONE', ( #7267 ), #6593, .T. ) ;
#3420 = CIRCLE ( 'NONE', #1744, 140.0000000000000000 ) ;
#3421 = LINE ( 'NONE', #564, #265 ) ;
#3422 = CARTESIAN_POINT ( 'NONE',  ( 14.97072768011073940, -34.32654753528365177, 2.597518595105000383 ) ) ;
#3423 = DIRECTION ( 'NONE',  ( -1.850371707708594129E-14, -4.625929269271485795E-14, 1.000000000000000000 ) ) ;
#3424 = DIRECTION ( 'NONE',  ( 0.7411265327553918647, 0.6713653717953965705, 6.883823317368281823E-16 ) ) ;
#3425 = EDGE_CURVE ( 'NONE', #6921, #4300, #5466, .T. ) ;
#3426 = EDGE_CURVE ( 'NONE', #1547, #3496, #4946, .T. ) ;
#3427 = SURFACE_STYLE_USAGE ( .BOTH. , #5699 ) ;
#3428 = EDGE_LOOP ( 'NONE', ( #693, #2175 ) ) ;
#3429 = ORIENTED_EDGE ( 'NONE', *, *, #5654, .F. ) ;
#3430 = CARTESIAN_POINT ( 'NONE',  ( 17.99698676687863852, -40.34744519239936267, 3.503909830570486328 ) ) ;
#3431 = CARTESIAN_POINT ( 'NONE',  ( -40.82267254781529431, -94.88271315313488685, -3.001000000000096257 ) ) ;
#3432 = EDGE_CURVE ( 'NONE', #5578, #7025, #6123, .T. ) ;
#3433 = DIRECTION ( 'NONE',  ( -5.715354789860003484E-18, -9.999836672264337477E-16, 1.000000000000000000 ) ) ;
#3434 = CARTESIAN_POINT ( 'NONE',  ( 2.193175381750440245, -67.18695861934700986, -2.930484425198875087 ) ) ;
#3435 = DIRECTION ( 'NONE',  ( 0.9793199139485099236, 0.2023178344681530461, 2.079116908177651401E-16 ) ) ;
#3436 = ORIENTED_EDGE ( 'NONE', *, *, #6628, .F. ) ;
#3437 = DIRECTION ( 'NONE',  ( -5.715354789845005112E-18, -9.999836672264339449E-16, 1.000000000000000000 ) ) ;
#3438 = DIRECTION ( 'NONE',  ( -0.08966155106958693943, -0.9959722919136836383, 0.000000000000000000 ) ) ;
#3439 = CYLINDRICAL_SURFACE ( 'NONE', #4855, 3.299999999999998934 ) ;
#3440 = ADVANCED_FACE ( 'NONE', ( #5522 ), #3165, .T. ) ;
#3441 = CARTESIAN_POINT ( 'NONE',  ( 5.164426235684419275, -63.32698789961681030, 0.7537993011490951023 ) ) ;
#3442 = CARTESIAN_POINT ( 'NONE',  ( -8.617355793880991044, 7.615193964809154004, -2.999999999999993339 ) ) ;
#3443 = CARTESIAN_POINT ( 'NONE',  ( -14.63712380658832046, -35.33334692323139592, -3.626931576674818025 ) ) ;
#3444 = ORIENTED_EDGE ( 'NONE', *, *, #4416, .F. ) ;
#3445 = ORIENTED_EDGE ( 'NONE', *, *, #4170, .T. ) ;
#3446 = VERTEX_POINT ( 'NONE', #4340 ) ;
#3447 = ITEM_DEFINED_TRANSFORMATION ( 'NONE', 'NONE', #3404,  #751 ) ;
#3448 = LINE ( 'NONE', #5844, #1730 ) ;
#3449 = EDGE_LOOP ( 'NONE', ( #6815, #5042, #4423, #1484 ) ) ;
#3450 = LINE ( 'NONE', #5762, #1837 ) ;
#3451 = CARTESIAN_POINT ( 'NONE',  ( 6.180415987647270626, -62.45112898858806716, 0.6030958204723052551 ) ) ;
#3452 = CARTESIAN_POINT ( 'NONE',  ( 27.13735696382475027, -34.54264957135247016, -0.3997825902234797835 ) ) ;
#3453 = CARTESIAN_POINT ( 'NONE',  ( 4.756074659365879143, -62.80135681555328375, -3.311393743080873975 ) ) ;
#3454 = ORIENTED_EDGE ( 'NONE', *, *, #6726, .F. ) ;
#3455 = ORIENTED_EDGE ( 'NONE', *, *, #6379, .F. ) ;
#3456 = EDGE_CURVE ( 'NONE', #5486, #4359, #4254, .T. ) ;
#3457 = CARTESIAN_POINT ( 'NONE',  ( -105.7473861751082040, -118.0666774205683822, 2.999999999999881428 ) ) ;
#3458 = DIRECTION ( 'NONE',  ( -0.2023178344681514362, 0.9793199139485103677, 9.781476007338052840E-16 ) ) ;
#3459 = DIRECTION ( 'NONE',  ( -5.715354789860003484E-18, -9.999836672264337477E-16, 1.000000000000000000 ) ) ;
#3460 = DIRECTION ( 'NONE',  ( -5.715354789860003484E-18, -9.999836672264337477E-16, 1.000000000000000000 ) ) ;
#3461 = DIRECTION ( 'NONE',  ( -5.715354789845005112E-18, -9.999836672264339449E-16, 1.000000000000000000 ) ) ;
#3462 = LINE ( 'NONE', #6370, #3005 ) ;
#3463 = ORIENTED_EDGE ( 'NONE', *, *, #5743, .F. ) ;
#3464 = CARTESIAN_POINT ( 'NONE',  ( 18.52223854178785345, -40.03305638412986411, 3.974049037550727803 ) ) ;
#3465 = CYLINDRICAL_SURFACE ( 'NONE', #6309, 11.50000000000000178 ) ;
#3466 = CARTESIAN_POINT ( 'NONE',  ( -0.004658654679648590799, -66.23339599434021352, 1.140748123765403355 ) ) ;
#3467 = CARTESIAN_POINT ( 'NONE',  ( 6.272193759149150338, -58.74577472516177323, -1.694429590687548837 ) ) ;
#3468 = CARTESIAN_POINT ( 'NONE',  ( -17.04733905648494030, -8.234069079964157822, -3.000000000000009326 ) ) ;
#3469 = ORIENTED_EDGE ( 'NONE', *, *, #7135, .T. ) ;
#3470 = CARTESIAN_POINT ( 'NONE',  ( -5.104186137876693508, -62.13399138291284629, 3.298500478949792480 ) ) ;
#3471 = EDGE_CURVE ( 'NONE', #3938, #4842, #3878, .T. ) ;
#3472 = ADVANCED_FACE ( 'NONE', ( #6781 ), #3352, .T. ) ;
#3473 = DIRECTION ( 'NONE',  ( -0.9999836672264335036, 0.005715354789845003385, 1.110223024625156047E-16 ) ) ;
#3474 = DIRECTION ( 'NONE',  ( 0.9999836672264332815, -0.005715354789845002517, 0.000000000000000000 ) ) ;
#3475 = DIRECTION ( 'NONE',  ( -0.5224671166576538850, 0.8526594349512809368, 0.000000000000000000 ) ) ;
#3476 = CARTESIAN_POINT ( 'NONE',  ( 4.348279337280104961, -63.27746244242579365, -1.677170969482009832 ) ) ;
#3477 = CARTESIAN_POINT ( 'NONE',  ( 27.08917652808902687, -34.57010060277283969, 3.436818098114547748 ) ) ;
#3478 = CYLINDRICAL_SURFACE ( 'NONE', #5065, 0.9999999999999998890 ) ;
#3479 = EDGE_LOOP ( 'NONE', ( #3931, #5729, #3252, #2034 ) ) ;
#3480 = VERTEX_POINT ( 'NONE', #1064 ) ;
#3481 = CIRCLE ( 'NONE', #2031, 5.000000000000000000 ) ;
#3482 = CARTESIAN_POINT ( 'NONE',  ( 14.02750760687355935, -37.17441268192290238, 0.4975185951050001831 ) ) ;
#3483 = VERTEX_POINT ( 'NONE', #4042 ) ;
#3484 = CARTESIAN_POINT ( 'NONE',  ( 6.071255580768259108, -56.77894568653594121, -1.427178034550365959 ) ) ;
#3485 = CARTESIAN_POINT ( 'NONE',  ( 27.40755238667390614, -34.38870444966534734, -0.8044411694303389426 ) ) ;
#3486 = CARTESIAN_POINT ( 'NONE',  ( -5.310432382237169513, -59.25281681403794209, -2.339912608914485936 ) ) ;
#3487 = VECTOR ( 'NONE', #6970, 1000.000000000000227 ) ;
#3488 = ORIENTED_EDGE ( 'NONE', *, *, #5324, .T. ) ;
#3489 = CARTESIAN_POINT ( 'NONE',  ( -35.54168210215660650, 14.82156649444490348, -0.7500000000019999558 ) ) ;
#3490 = CARTESIAN_POINT ( 'NONE',  ( -13.49899450467539985, -35.75040780681265318, -0.4662714048949997969 ) ) ;
#3491 = AXIS2_PLACEMENT_3D ( 'NONE', #3443, #1195, #2385 ) ;
#3492 = DIRECTION ( 'NONE',  ( -5.715354789860003484E-18, -9.999836672264337477E-16, 1.000000000000000000 ) ) ;
#3493 = PLANE ( 'NONE',  #1008 ) ;
#3494 = CARTESIAN_POINT ( 'NONE',  ( -6.216708800954390490, -58.75440211775612909, 1.606470739968075545 ) ) ;
#3495 = LINE ( 'NONE', #1696, #2045 ) ;
#3496 = VERTEX_POINT ( 'NONE', #606 ) ;
#3497 = EDGE_LOOP ( 'NONE', ( #66, #5282, #7173, #6764, #1328 ) ) ;
#3498 = CARTESIAN_POINT ( 'NONE',  ( 2.576047814891095022, -64.81584722952422339, -0.4432308004904150223 ) ) ;
#3499 = FACE_OUTER_BOUND ( 'NONE', #5471, .T. ) ;
#3500 = CLOSED_SHELL ( 'NONE', ( #5646, #4777, #1191 ) ) ;
#3501 = DIRECTION ( 'NONE',  ( -5.715354789845005112E-18, -9.999836672264339449E-16, 1.000000000000000000 ) ) ;
#3502 = CARTESIAN_POINT ( 'NONE',  ( 5.544705546025709531, -62.26256661181761842, 0.7210154936787926960 ) ) ;
#3503 = CARTESIAN_POINT ( 'NONE',  ( -5.982481740117790103, -62.36145600051965232, 1.442409191505919619 ) ) ;
#3504 = EDGE_CURVE ( 'NONE', #936, #4310, #5830, .T. ) ;
#3505 = CARTESIAN_POINT ( 'NONE',  ( -15.08175531864075047, -33.99084820126180517, -5.041145139047909396 ) ) ;
#3506 = ORIENTED_EDGE ( 'NONE', *, *, #714, .F. ) ;
#3507 = VECTOR ( 'NONE', #6460, 1000.000000000000000 ) ;
#3508 = CARTESIAN_POINT ( 'NONE',  ( -5.094026379717228714, -62.13064902308300219, 3.289882701435055345 ) ) ;
#3509 = AXIS2_PLACEMENT_3D ( 'NONE', #1689, #4561, #3984 ) ;
#3510 = FACE_OUTER_BOUND ( 'NONE', #6696, .T. ) ;
#3511 = CARTESIAN_POINT ( 'NONE',  ( 41.70778007397900211, -94.98992620957551480, 3.999999999999905409 ) ) ;
#3512 = VECTOR ( 'NONE', #6155, 1000.000000000000000 ) ;
#3513 = CARTESIAN_POINT ( 'NONE',  ( -5.624257096981370552, -62.27449455720285698, -0.5715238816199899041 ) ) ;
#3514 = AXIS2_PLACEMENT_3D ( 'NONE', #1691, #2397, #1735 ) ;
#3515 = CARTESIAN_POINT ( 'NONE',  ( -5.524241737545620090, -57.12730840725460979, 1.694319224817255165 ) ) ;
#3516 = CARTESIAN_POINT ( 'NONE',  ( -14.49899450467539985, -35.75040780681265318, -2.566271404894997499 ) ) ;
#3517 = VERTEX_POINT ( 'NONE', #2782 ) ;
#3518 = EDGE_CURVE ( 'NONE', #4029, #2611, #1183, .T. ) ;
#3519 = ORIENTED_EDGE ( 'NONE', *, *, #3387, .T. ) ;
#3520 = ORIENTED_EDGE ( 'NONE', *, *, #27, .T. ) ;
#3521 = EDGE_LOOP ( 'NONE', ( #4696, #1061, #6283, #65 ) ) ;
#3522 = VECTOR ( 'NONE', #3218, 1000.000000000000000 ) ;
#3523 = CARTESIAN_POINT ( 'NONE',  ( 26.67188031194815068, 24.16129507000589527, -2.993845543551515664 ) ) ;
#3524 = CARTESIAN_POINT ( 'NONE',  ( 14.29543924104632779, -35.83228874779774742, 2.999999999999964473 ) ) ;
#3525 = CARTESIAN_POINT ( 'NONE',  ( -1.409024882572649906, -54.10038288851608712, -0.1041033434293599513 ) ) ;
#3526 = CARTESIAN_POINT ( 'NONE',  ( -13.12771516100364799, 4.746262909141762520, 16.32566479563440609 ) ) ;
#3527 = CIRCLE ( 'NONE', #4499, 6.300000000000002487 ) ;
#3528 = ADVANCED_FACE ( 'NONE', ( #6308 ), #7418, .F. ) ;
#3529 = AXIS2_PLACEMENT_3D ( 'NONE', #6945, #1709, #5223 ) ;
#3530 = B_SPLINE_CURVE_WITH_KNOTS ( 'NONE', 1,
 ( #5356, #3644 ),
 .UNSPECIFIED., .F., .F.,
 ( 2, 2 ),
 ( 0.000000000000000000, 1.000000000000000000 ),
 .UNSPECIFIED. ) ;
#3531 = EDGE_LOOP ( 'NONE', ( #7162, #2515, #172, #1612 ) ) ;
#3532 = CIRCLE ( 'NONE', #6773, 5.000000000000001776 ) ;
#3533 = B_SPLINE_CURVE_WITH_KNOTS ( 'NONE', 3,
 ( #6586, #3114, #6556, #907 ),
 .UNSPECIFIED., .F., .F.,
 ( 4, 4 ),
 ( 0.000000000000000000, 1.000000000000000000 ),
 .UNSPECIFIED. ) ;
#3534 = VERTEX_POINT ( 'NONE', #2227 ) ;
#3535 = AXIS2_PLACEMENT_3D ( 'NONE', #2763, #6286, #5686 ) ;
#3536 = LINE ( 'NONE', #2255, #4236 ) ;
#3537 = FACE_OUTER_BOUND ( 'NONE', #1278, .T. ) ;
#3538 = AXIS2_PLACEMENT_3D ( 'NONE', #2437, #7037, #4364 ) ;
#3539 = DIRECTION ( 'NONE',  ( -0.3144019573014849023, 0.9492899500389726519, 0.000000000000000000 ) ) ;
#3540 = CARTESIAN_POINT ( 'NONE',  ( 3.331090576803830139, -65.95739139720836874, 0.8111086825117052035 ) ) ;
#3541 = DIRECTION ( 'NONE',  ( -0.3536350175650657124, -0.3203478684871222115, -0.8788171126619652718 ) ) ;
#3542 = CIRCLE ( 'NONE', #2218, 4.000000000000000000 ) ;
#3543 = CARTESIAN_POINT ( 'NONE',  ( 12.87643844828394535, 18.94962249585221414, -2.729489053861940739 ) ) ;
#3544 = DIRECTION ( 'NONE',  ( -0.9999836672264333925, 0.005715354789844971292, -3.141587852546554631E-32 ) ) ;
#3545 = LINE ( 'NONE', #1703, #366 ) ;
#3546 = ORIENTED_EDGE ( 'NONE', *, *, #1641, .F. ) ;
#3547 = DIRECTION ( 'NONE',  ( 0.9999836672264333925, -0.005715354789844381486, 0.000000000000000000 ) ) ;
#3548 = ADVANCED_FACE ( 'NONE', ( #4534 ), #2347, .F. ) ;
#3549 = CARTESIAN_POINT ( 'NONE',  ( 18.21884925479887940, -40.21464179917847304, -0.7992328572925022634 ) ) ;
#3550 = CARTESIAN_POINT ( 'NONE',  ( -5.076816837522959425, -57.40733507789485657, 1.813788655352380541 ) ) ;
#3551 = CARTESIAN_POINT ( 'NONE',  ( -5.996378862946620814, -62.15612413928192836, 3.522786485084270058 ) ) ;
#3552 = CARTESIAN_POINT ( 'NONE',  ( -17.02208700381124729, 2.051506657828173541, 3.000000000000002220 ) ) ;
#3553 = ORIENTED_EDGE ( 'NONE', *, *, #3774, .F. ) ;
#3554 = ORIENTED_EDGE ( 'NONE', *, *, #979, .T. ) ;
#3555 = B_SPLINE_SURFACE_WITH_KNOTS ( 'NONE', 1, 3, ( 
 ( #3626, #5948, #775, #5498 ),
 ( #6681, #3732, #3286, #5603 ) ),
 .UNSPECIFIED., .F., .F., .F.,
 ( 2, 2 ),
 ( 4, 4 ),
 ( 0.000000000000000000, 1.000000000000000000 ),
 ( 0.000000000000000000, 1.000000000000000000 ),
 .UNSPECIFIED. ) ;
#3556 = EDGE_CURVE ( 'NONE', #3706, #6490, #1373, .T. ) ;
#3557 = ADVANCED_FACE ( 'NONE', ( #5664 ), #1149, .F. ) ;
#3558 = FACE_OUTER_BOUND ( 'NONE', #5591, .T. ) ;
#3559 = CARTESIAN_POINT ( 'NONE',  ( -105.7473861751082040, -118.0666774205683822, -1.188285581044112860E-13 ) ) ;
#3560 = CARTESIAN_POINT ( 'NONE',  ( 1.915558458284230214, -54.23376817553720031, 0.07315972318039029587 ) ) ;
#3561 = PRODUCT_RELATED_PRODUCT_CATEGORY ( 'part', '', ( #846 ) ) ;
#3562 = CARTESIAN_POINT ( 'NONE',  ( 27.74785688037308518, -34.19481435285785409, -4.220975948576798359E-14 ) ) ;
#3563 = VERTEX_POINT ( 'NONE', #1103 ) ;
#3564 = ADVANCED_FACE ( 'NONE', ( #573 ), #4569, .F. ) ;
#3565 = ADVANCED_FACE ( 'NONE', ( #2858 ), #3465, .T. ) ;
#3566 = DIRECTION ( 'NONE',  ( -5.715354789860003484E-18, -9.999836672264337477E-16, 1.000000000000000000 ) ) ;
#3567 = DIRECTION ( 'NONE',  ( -5.715354789860003484E-18, -9.999836672264337477E-16, 1.000000000000000000 ) ) ;
#3568 = CARTESIAN_POINT ( 'NONE',  ( 6.641713594241586804, -62.65488624492035541, -2.690269354371802368 ) ) ;
#3569 = CARTESIAN_POINT ( 'NONE',  ( -5.996378862946620814, -62.15612413928192836, 3.522786485084270058 ) ) ;
#3570 = CARTESIAN_POINT ( 'NONE',  ( -6.223557239263538321, -60.98460414740468138, 1.486641091859571162 ) ) ;
#3571 = VERTEX_POINT ( 'NONE', #6903 ) ;
#3572 = ADVANCED_FACE ( 'NONE', ( #6939 ), #1746, .T. ) ;
#3573 = CARTESIAN_POINT ( 'NONE',  ( 1.277257345132870148, -65.35512402512885899, -0.3535023904437397113 ) ) ;
#3574 = CARTESIAN_POINT ( 'NONE',  ( -19.65288587824389310, 14.48569475295020226, -2.993845543551517441 ) ) ;
#3575 = FACE_OUTER_BOUND ( 'NONE', #594, .T. ) ;
#3576 = CARTESIAN_POINT ( 'NONE',  ( 0.8260371565349720058, -66.17440364758674320, -3.107556223232925241 ) ) ;
#3577 = DIRECTION ( 'NONE',  ( -0.4328040977884316520, 0.5819352847797604200, 0.6884997728872834788 ) ) ;
#3578 = ORIENTED_EDGE ( 'NONE', *, *, #1774, .F. ) ;
#3579 = CARTESIAN_POINT ( 'NONE',  ( -20.89962323070193406, -41.21687045383659154, -4.133564602976221858E-14 ) ) ;
#3580 = DIRECTION ( 'NONE',  ( -5.715354789860003484E-18, -9.999836672264337477E-16, 1.000000000000000000 ) ) ;
#3581 = CARTESIAN_POINT ( 'NONE',  ( 18.31450470689560461, -40.15738718825951992, -0.8737133221916458803 ) ) ;
#3582 = UNCERTAINTY_MEASURE_WITH_UNIT (LENGTH_MEASURE( 1.000000000000000082E-05 ), #2815, 'distance_accuracy_value', 'NONE');
#3583 = CARTESIAN_POINT ( 'NONE',  ( -1.556563313654149905, -55.35434594439572464, -0.3959639196582302456 ) ) ;
#3584 = CARTESIAN_POINT ( 'NONE',  ( 94.42889356597736139, -103.2882618349535591, -3.000000000000103917 ) ) ;
#3585 = FACE_BOUND ( 'NONE', #1163, .T. ) ;
#3586 = VERTEX_POINT ( 'NONE', #5778 ) ;
#3587 = VERTEX_POINT ( 'NONE', #4498 ) ;
#3588 = ORIENTED_CLOSED_SHELL ( 'NONE', *, #4472, .F. );
#3589 = VERTEX_POINT ( 'NONE', #2893 ) ;
#3590 = ORIENTED_EDGE ( 'NONE', *, *, #6211, .F. ) ;
#3591 = DIRECTION ( 'NONE',  ( -0.9999836672264335036, 0.005715354789845008589, 0.000000000000000000 ) ) ;
#3592 = DIRECTION ( 'NONE',  ( -0.9999836672264333925, 0.005715354789845005987, 4.554564057672517313E-33 ) ) ;
#3593 = CARTESIAN_POINT ( 'NONE',  ( 2.193175381750440245, -67.18695861934700986, -2.930484425198875087 ) ) ;
#3594 = DIRECTION ( 'NONE',  ( -5.715354789845005112E-18, -9.999836672264339449E-16, 1.000000000000000000 ) ) ;
#3595 = ORIENTED_EDGE ( 'NONE', *, *, #5925, .F. ) ;
#3596 = CIRCLE ( 'NONE', #5543, 0.7499999999999893419 ) ;
#3597 = DIRECTION ( 'NONE',  ( 0.000000000000000000, 0.000000000000000000, 1.000000000000000000 ) ) ;
#3598 = DIRECTION ( 'NONE',  ( 0.4039838799357199361, 0.9147661038495479291, 4.432239818696054780E-17 ) ) ;
#3599 = CARTESIAN_POINT ( 'NONE',  ( 10.07902270299396008, 17.77910117033601978, 2.236547809770398132 ) ) ;
#3600 = AXIS2_PLACEMENT_3D ( 'NONE', #6940, #543, #4108 ) ;
#3601 = CARTESIAN_POINT ( 'NONE',  ( 6.061184043039538949, -62.50365188168748176, -3.430634321730453351 ) ) ;
#3602 = CARTESIAN_POINT ( 'NONE',  ( -10.41850315652351533, -32.21925899276746463, -3.000000000000032863 ) ) ;
#3603 = FACE_OUTER_BOUND ( 'NONE', #6712, .T. ) ;
#3604 = EDGE_CURVE ( 'NONE', #2388, #7211, #5953, .T. ) ;
#3605 = ADVANCED_FACE ( 'NONE', ( #5630 ), #4151, .T. ) ;
#3606 = CONICAL_SURFACE ( 'NONE', #369, 0.7500000000000002220, 1.029744258676651425 ) ;
#3607 = CARTESIAN_POINT ( 'NONE',  ( 5.191094514348209898, -57.61090315545595786, 2.520404771314449732 ) ) ;
#3608 = CARTESIAN_POINT ( 'NONE',  ( 13.14859132361182148, 19.41219719266456423, 0.4060579846639996715 ) ) ;
#3609 = CARTESIAN_POINT ( 'NONE',  ( -32.92087242456759100, 14.53869105662955619, 0.006154456448484012937 ) ) ;
#3610 = CARTESIAN_POINT ( 'NONE',  ( -5.408374332777167837, -58.11854958432094520, -2.399418114313899508 ) ) ;
#3611 = CIRCLE ( 'NONE', #4595, 2.999999999999999556 ) ;
#3612 = PRODUCT_DEFINITION_SHAPE ( 'NONE', 'NONE',  #7449 ) ;
#3613 = ORIENTED_EDGE ( 'NONE', *, *, #3987, .T. ) ;
#3614 = FACE_OUTER_BOUND ( 'NONE', #1463, .T. ) ;
#3615 = CLOSED_SHELL ( 'NONE', ( #5776, #2777, #6140, #3640, #1321, #7424, #3899, #1681, #2357, #3792, #2087, #3944, #2086, #7095, #5267, #4112, #3283, #6741, #3284, #2635, #3236, #2194, #6936, #4030, #7000, #706 ) ) ;
#3616 = DIRECTION ( 'NONE',  ( 0.3128463504745289669, 0.9445772445362837777, 0.09950371902099817978 ) ) ;
#3617 = CARTESIAN_POINT ( 'NONE',  ( 18.52082317230821928, -40.03390347989001441, -0.9734914404586040293 ) ) ;
#3618 = CARTESIAN_POINT ( 'NONE',  ( 6.187144687173720570, -58.64655194120005177, 0.3691021985165400809 ) ) ;
#3619 = CARTESIAN_POINT ( 'NONE',  ( -4.780177894917470027, -57.84320307688069107, -2.250545046436859931 ) ) ;
#3620 = CARTESIAN_POINT ( 'NONE',  ( 1.785462125252589960, -54.25404267560509908, 2.136629312307830375 ) ) ;
#3621 = LINE ( 'NONE', #5403, #3985 ) ;
#3622 = ADVANCED_FACE ( 'NONE', ( #87 ), #6253, .T. ) ;
#3623 = CIRCLE ( 'NONE', #3995, 6.500000000000001776 ) ;
#3624 = EDGE_LOOP ( 'NONE', ( #7321, #4860, #259, #2443 ) ) ;
#3625 = ORIENTED_EDGE ( 'NONE', *, *, #7316, .F. ) ;
#3626 = CARTESIAN_POINT ( 'NONE',  ( -15.07233531785332659, 13.90759097395377886, 2.236547809770393691 ) ) ;
#3627 =( GEOMETRIC_REPRESENTATION_CONTEXT ( 3 ) GLOBAL_UNCERTAINTY_ASSIGNED_CONTEXT ( ( #2678 ) ) GLOBAL_UNIT_ASSIGNED_CONTEXT ( ( #2346, #4654, #2377 ) ) REPRESENTATION_CONTEXT ( 'NONE', 'WORKASPACE' ) );
#3628 = AXIS2_PLACEMENT_3D ( 'NONE', #3406, #1159, #6916 ) ;
#3629 = DIRECTION ( 'NONE',  ( -5.715354789860004255E-18, -9.999836672264337477E-16, 1.000000000000000000 ) ) ;
#3630 = CARTESIAN_POINT ( 'NONE',  ( -3.018293710664720297, -66.19764165108277609, -3.019563749174228207 ) ) ;
#3631 = VECTOR ( 'NONE', #2165, 1000.000000000000000 ) ;
#3632 = ORIENTED_EDGE ( 'NONE', *, *, #1951, .T. ) ;
#3633 = VECTOR ( 'NONE', #4887, 1000.000000000000114 ) ;
#3634 = ORIENTED_EDGE ( 'NONE', *, *, #5545, .T. ) ;
#3635 = VERTEX_POINT ( 'NONE', #1948 ) ;
#3636 = VECTOR ( 'NONE', #6753, 1000.000000000000000 ) ;
#3637 = PRESENTATION_LAYER_ASSIGNMENT (  '', '', ( #6412 ) ) ;
#3638 =( NAMED_UNIT ( * ) SI_UNIT ( $, .STERADIAN. ) SOLID_ANGLE_UNIT ( ) );
#3639 = DIRECTION ( 'NONE',  ( -2.712383034095203713E-15, 1.348591164987489727E-15, -1.000000000000000000 ) ) ;
#3640 = ADVANCED_FACE ( 'NONE', ( #4107 ), #1074, .T. ) ;
#3641 = AXIS2_PLACEMENT_3D ( 'NONE', #4384, #7303, #1516 ) ;
#3642 = DIRECTION ( 'NONE',  ( 0.9492883822130744331, -0.3144066910790611624, 0.000000000000000000 ) ) ;
#3643 = AXIS2_PLACEMENT_3D ( 'NONE', #5381, #213, #3591 ) ;
#3644 = CARTESIAN_POINT ( 'NONE',  ( 9.018117650298766108, 16.81805756487467107, -0.3999035282154979054 ) ) ;
#3645 = DIRECTION ( 'NONE',  ( -5.715354789860003484E-18, -9.999836672264337477E-16, 1.000000000000000000 ) ) ;
#3646 = VERTEX_POINT ( 'NONE', #1219 ) ;
#3647 = CIRCLE ( 'NONE', #4626, 5.000000000000000000 ) ;
#3648 = FACE_OUTER_BOUND ( 'NONE', #4327, .T. ) ;
#3649 = CARTESIAN_POINT ( 'NONE',  ( -5.065438427596520299, -62.07564176717611559, -0.9259012332463799622 ) ) ;
#3650 = AXIS2_PLACEMENT_3D ( 'NONE', #3008, #2975, #4110 ) ;
#3651 = AXIS2_PLACEMENT_3D ( 'NONE', #2641, #1550, #4948 ) ;
#3652 = EDGE_CURVE ( 'NONE', #6398, #2388, #6721, .T. ) ;
#3653 = EDGE_CURVE ( 'NONE', #3224, #2318, #5538, .T. ) ;
#3654 = DIRECTION ( 'NONE',  ( 5.715354789845005112E-18, 9.999836672264339449E-16, -1.000000000000000000 ) ) ;
#3655 = CARTESIAN_POINT ( 'NONE',  ( 0.9632665884170439341, -54.73762666295851886, -1.953671419500376816 ) ) ;
#3656 = AXIS2_PLACEMENT_3D ( 'NONE', #5087, #7373, #2851 ) ;
#3657 = VERTEX_POINT ( 'NONE', #2486 ) ;
#3658 = DIRECTION ( 'NONE',  ( -0.6713653717953944611, 0.7411265327553937521, -9.186864590530470220E-16 ) ) ;
#3659 = EDGE_CURVE ( 'NONE', #6227, #2912, #1812, .T. ) ;
#3660 = FACE_OUTER_BOUND ( 'NONE', #3531, .T. ) ;
#3661 = CARTESIAN_POINT ( 'NONE',  ( 18.07563673267965854, -39.70560758510323041, -0.1308779909158750421 ) ) ;
#3662 = DIRECTION ( 'NONE',  ( 0.3144066910790610514, 0.9492883822130742111, 0.000000000000000000 ) ) ;
#3663 = DIRECTION ( 'NONE',  ( -5.715354789860003484E-18, -9.999836672264337477E-16, 1.000000000000000000 ) ) ;
#3664 = DIRECTION ( 'NONE',  ( 0.000000000000000000, 0.000000000000000000, 1.000000000000000000 ) ) ;
#3665 = EDGE_LOOP ( 'NONE', ( #3673, #7189, #2890, #1834 ) ) ;
#3666 = VERTEX_POINT ( 'NONE', #790 ) ;
#3667 = FACE_BOUND ( 'NONE', #2600, .T. ) ;
#3668 = ADVANCED_FACE ( 'NONE', ( #3575 ), #5859, .T. ) ;
#3669 = DIRECTION ( 'NONE',  ( 0.7411265327553916427, 0.6713653717953966815, 6.883823317368282809E-16 ) ) ;
#3670 = CARTESIAN_POINT ( 'NONE',  ( 5.271413390890690387, -61.79997272665566044, -1.279516964844005900 ) ) ;
#3671 = VERTEX_POINT ( 'NONE', #4790 ) ;
#3672 = ORIENTED_EDGE ( 'NONE', *, *, #5410, .F. ) ;
#3673 = ORIENTED_EDGE ( 'NONE', *, *, #2398, .T. ) ;
#3674 = DIRECTION ( 'NONE',  ( -0.8748844214391259255, 0.1369338178966306718, -0.4645711771509057897 ) ) ;
#3675 = CARTESIAN_POINT ( 'NONE',  ( -105.7473861751082040, -118.0666774205683822, -1.186117176699141851E-13 ) ) ;
#3676 = CYLINDRICAL_SURFACE ( 'NONE', #4977, 2.999999999999999556 ) ;
#3677 = CARTESIAN_POINT ( 'NONE',  ( -3.498019654714389581, -55.03494779767484602, -0.2490962732230048438 ) ) ;
#3678 = ORIENTED_EDGE ( 'NONE', *, *, #4253, .F. ) ;
#3679 = EDGE_CURVE ( 'NONE', #7067, #5349, #382, .T. ) ;
#3680 = DIRECTION ( 'NONE',  ( 0.9999836672264335036, -0.005715354789845041548, 0.000000000000000000 ) ) ;
#3681 = CARTESIAN_POINT ( 'NONE',  ( 5.768687865266859838, -59.13854474313614418, 2.609246528188839509 ) ) ;
#3682 = CARTESIAN_POINT ( 'NONE',  ( -31.91091272472834817, 16.82560631625344172, -2.993845543551523214 ) ) ;
#3683 = DIRECTION ( 'NONE',  ( -0.9721221936972339606, -0.2344748185227520099, 0.000000000000000000 ) ) ;
#3684 = CARTESIAN_POINT ( 'NONE',  ( 14.07443455944474131, -37.03272609524245240, -0.9950371902099899302 ) ) ;
#3685 = ORIENTED_EDGE ( 'NONE', *, *, #1775, .F. ) ;
#3686 = EDGE_CURVE ( 'NONE', #4811, #4478, #4754, .T. ) ;
#3687 = DIRECTION ( 'NONE',  ( 0.9492899500389727629, 0.3144019573014849023, 0.000000000000000000 ) ) ;
#3688 = LINE ( 'NONE', #5369, #56 ) ;
#3689 = CARTESIAN_POINT ( 'NONE',  ( 18.44199058758350063, -39.49687574139178992, -0.4999999711863141738 ) ) ;
#3690 = CARTESIAN_POINT ( 'NONE',  ( -2.887726905928315269, -66.20272978495717098, -0.9560320787877147897 ) ) ;
#3691 = APPLICATION_CONTEXT ( 'automotive_design' ) ;
#3692 = CARTESIAN_POINT ( 'NONE',  ( 1.830733139179690161, -67.16965779809959258, 0.7798461408577649356 ) ) ;
#3693 = CARTESIAN_POINT ( 'NONE',  ( -14.49899450467539985, -35.75040780681265318, -2.566271404894997499 ) ) ;
#3694 = ORIENTED_EDGE ( 'NONE', *, *, #4570, .F. ) ;
#3695 = EDGE_CURVE ( 'NONE', #901, #2204, #5894, .T. ) ;
#3696 = EDGE_CURVE ( 'NONE', #216, #909, #2522, .T. ) ;
#3697 = ORIENTED_EDGE ( 'NONE', *, *, #2454, .T. ) ;
#3698 = EDGE_LOOP ( 'NONE', ( #3798, #5346, #7228, #1724 ) ) ;
#3699 = CARTESIAN_POINT ( 'NONE',  ( 104.0973215944787711, -119.5240462704291389, -1.189271409856590718E-13 ) ) ;
#3700 = DIRECTION ( 'NONE',  ( 0.9999836672264332815, -0.005715354789860001804, 0.000000000000000000 ) ) ;
#3701 = CARTESIAN_POINT ( 'NONE',  ( 5.944105978113960020, -62.47685828501489169, -3.593838583070729786 ) ) ;
#3702 = CARTESIAN_POINT ( 'NONE',  ( 5.093888048015757342, -64.05487131086009356, 2.771559435373996738 ) ) ;
#3703 = ORIENTED_EDGE ( 'NONE', *, *, #5147, .F. ) ;
#3704 = ORIENTED_EDGE ( 'NONE', *, *, #4171, .T. ) ;
#3705 = EDGE_CURVE ( 'NONE', #4811, #1688, #7110, .T. ) ;
#3706 = VERTEX_POINT ( 'NONE', #7074 ) ;
#3707 = ORIENTED_EDGE ( 'NONE', *, *, #4632, .F. ) ;
#3708 = DIRECTION ( 'NONE',  ( 0.05111947575938272093, -0.9986925448795970217, -9.983840675197636492E-16 ) ) ;
#3709 = DIRECTION ( 'NONE',  ( -0.9721221936972339606, -0.2344748185227520376, 0.000000000000000000 ) ) ;
#3710 = CARTESIAN_POINT ( 'NONE',  ( 9.018117650298766108, 16.81805756487467107, -0.3999035282154979054 ) ) ;
#3711 = CARTESIAN_POINT ( 'NONE',  ( -1.735723365167664900, -67.19411771835910940, 0.9573769032209800134 ) ) ;
#3712 = VERTEX_POINT ( 'NONE', #6373 ) ;
#3713 = CARTESIAN_POINT ( 'NONE',  ( 43.95483829995806957, -94.87490738911687060, 3.999999999999905409 ) ) ;
#3714 = CARTESIAN_POINT ( 'NONE',  ( 3.069422284440780135, -65.49896014417400636, 0.9299900502622647780 ) ) ;
#3715 = VECTOR ( 'NONE', #7268, 1000.000000000000114 ) ;
#3716 = CYLINDRICAL_SURFACE ( 'NONE', #480, 1.000000000000001332 ) ;
#3717 = CARTESIAN_POINT ( 'NONE',  ( -5.570007062648755891, -62.18452688224461866, -2.635462372538256215 ) ) ;
#3718 = CIRCLE ( 'NONE', #2760, 147.0000000000000284 ) ;
#3719 = EDGE_LOOP ( 'NONE', ( #5944, #4813, #4631, #1024, #546, #6420, #7201, #6153 ) ) ;
#3720 = CARTESIAN_POINT ( 'NONE',  ( 43.95483829995806957, -94.87490738911687060, 3.999999999999905409 ) ) ;
#3721 = AXIS2_PLACEMENT_3D ( 'NONE', #3090, #1962, #1920 ) ;
#3722 = DIRECTION ( 'NONE',  ( 5.715354789860003484E-18, 9.999836672264337477E-16, -1.000000000000000000 ) ) ;
#3723 = DIRECTION ( 'NONE',  ( 0.7411265327553913096, 0.6713653717953970146, 6.755902076156640294E-16 ) ) ;
#3724 = EDGE_CURVE ( 'NONE', #5957, #901, #1324, .T. ) ;
#3725 = CARTESIAN_POINT ( 'NONE',  ( 38.49686355599224896, -95.49243502991532750, 2.999999999999904521 ) ) ;
#3726 = DIRECTION ( 'NONE',  ( 0.5297244269785086335, 0.8481698128690332572, 8.511835229445635643E-16 ) ) ;
#3727 = CARTESIAN_POINT ( 'NONE',  ( -6.728394430327000464, -62.68905628767773663, 2.815217869383099814 ) ) ;
#3728 = DIRECTION ( 'NONE',  ( -0.8174211450113090249, -0.5760405121937176576, -5.807029557109402914E-16 ) ) ;
#3729 = VERTEX_POINT ( 'NONE', #4716 ) ;
#3730 = ORIENTED_EDGE ( 'NONE', *, *, #1314, .F. ) ;
#3731 = AXIS2_PLACEMENT_3D ( 'NONE', #3806, #3394, #7306 ) ;
#3732 = CARTESIAN_POINT ( 'NONE',  ( -13.25406850835028649, 13.28961593883099468, -0.1384896246987418478 ) ) ;
#3733 = CARTESIAN_POINT ( 'NONE',  ( 27.65533861039811114, -36.12687000486602784, -3.001370543551575842 ) ) ;
#3734 = EDGE_CURVE ( 'NONE', #7442, #1697, #6480, .T. ) ;
#3735 = EDGE_CURVE ( 'NONE', #6877, #5957, #3228, .T. ) ;
#3736 = VECTOR ( 'NONE', #6161, 1000.000000000000000 ) ;
#3737 = DIRECTION ( 'NONE',  ( -5.715354789845005112E-18, -9.999836672264339449E-16, 1.000000000000000000 ) ) ;
#3738 = CARTESIAN_POINT ( 'NONE',  ( -1.516811388151804829, -54.38796383586615235, 1.958561210572854483 ) ) ;
#3739 = ORIENTED_EDGE ( 'NONE', *, *, #2454, .F. ) ;
#3740 = ORIENTED_EDGE ( 'NONE', *, *, #942, .F. ) ;
#3741 = EDGE_LOOP ( 'NONE', ( #336, #5474, #3106, #519, #295, #2010 ) ) ;
#3742 = TOROIDAL_SURFACE ( 'NONE', #743, 1.500000000000000000, 1.000000000000000000 ) ;
#3743 = VECTOR ( 'NONE', #6005, 1000.000000000000114 ) ;
#3744 = APPLICATION_PROTOCOL_DEFINITION ( 'draft international standard', 'automotive_design', 1998, #2933 ) ;
#3745 = FACE_OUTER_BOUND ( 'NONE', #479, .T. ) ;
#3746 = ADVANCED_FACE ( 'NONE', ( #1361 ), #3716, .T. ) ;
#3747 = PLANE ( 'NONE',  #4873 ) ;
#3748 = CARTESIAN_POINT ( 'NONE',  ( -3.132958547045754827, -66.67000521241658362, -1.075502346145061683 ) ) ;
#3749 = AXIS2_PLACEMENT_3D ( 'NONE', #6780, #2178, #3313 ) ;
#3750 = AXIS2_PLACEMENT_3D ( 'NONE', #5913, #1933, #1902 ) ;
#3751 = ORIENTED_EDGE ( 'NONE', *, *, #4497, .T. ) ;
#3752 = EDGE_LOOP ( 'NONE', ( #5108, #5628, #5941, #4167 ) ) ;
#3753 = CYLINDRICAL_SURFACE ( 'NONE', #4732, 0.7499999999999997780 ) ;
#3754 = AXIS2_PLACEMENT_3D ( 'NONE', #6247, #3371, #5124 ) ;
#3755 = CARTESIAN_POINT ( 'NONE',  ( -5.624257096981370552, -62.27449455720285698, -0.5715238816199899041 ) ) ;
#3756 = AXIS2_PLACEMENT_3D ( 'NONE', #2012, #6722, #1010 ) ;
#3757 = ORIENTED_EDGE ( 'NONE', *, *, #6221, .F. ) ;
#3758 = CIRCLE ( 'NONE', #7368, 1.000000000000000000 ) ;
#3759 = CARTESIAN_POINT ( 'NONE',  ( 43.95483829995806957, -94.87490738911687060, 2.999999999999905409 ) ) ;
#3760 = CARTESIAN_POINT ( 'NONE',  ( -5.565225078471084608, -62.28720617293075179, 1.537195128485716378 ) ) ;
#3761 = CIRCLE ( 'NONE', #3408, 5.000000000000000000 ) ;
#3762 = ORIENTED_EDGE ( 'NONE', *, *, #2215, .F. ) ;
#3763 = AXIS2_PLACEMENT_3D ( 'NONE', #3981, #7324, #1050 ) ;
#3764 = CARTESIAN_POINT ( 'NONE',  ( -15.52817266570582611, -38.02681526409561741, -3.811494319675517002E-14 ) ) ;
#3765 = PLANE ( 'NONE',  #6431 ) ;
#3766 = DIRECTION ( 'NONE',  ( -0.9147661038495521479, 0.4039838799357104993, 3.987490689252507167E-16 ) ) ;
#3767 = CARTESIAN_POINT ( 'NONE',  ( 5.676184037656430093, -63.13711808556965366, -1.485967351095627720 ) ) ;
#3768 = AXIS2_PLACEMENT_3D ( 'NONE', #7070, #3492, #781 ) ;
#3769 = DIRECTION ( 'NONE',  ( 5.715354789845005112E-18, 9.999836672264339449E-16, -1.000000000000000000 ) ) ;
#3770 = CARTESIAN_POINT ( 'NONE',  ( 3.219971992657300053, -66.62470095071212484, 2.812725188592500203 ) ) ;
#3771 = DIRECTION ( 'NONE',  ( 0.3144066910790613845, 0.9492883822130742111, 0.000000000000000000 ) ) ;
#3772 = ORIENTED_EDGE ( 'NONE', *, *, #4653, .T. ) ;
#3773 = CARTESIAN_POINT ( 'NONE',  ( -95.86211798318534250, -102.0316339954322018, -1.027823659516258203E-13 ) ) ;
#3774 = EDGE_CURVE ( 'NONE', #1643, #2855, #7199, .T. ) ;
#3775 = AXIS2_PLACEMENT_3D ( 'NONE', #3675, #896, #6545 ) ;
#3776 = LINE ( 'NONE', #5027, #3278 ) ;
#3777 = DIRECTION ( 'NONE',  ( -5.715354789845005112E-18, -9.999836672264339449E-16, 1.000000000000000000 ) ) ;
#3778 = CARTESIAN_POINT ( 'NONE',  ( 2.671142801832544933, -55.70169962949673703, -1.720663637103989618 ) ) ;
#3779 = FACE_OUTER_BOUND ( 'NONE', #2718, .T. ) ;
#3780 = CARTESIAN_POINT ( 'NONE',  ( 4.005285614311604903, -55.65094623700133525, 2.273239139415862198 ) ) ;
#3781 = ORIENTED_EDGE ( 'NONE', *, *, #5487, .F. ) ;
#3782 = VERTEX_POINT ( 'NONE', #3759 ) ;
#3783 = ORIENTED_EDGE ( 'NONE', *, *, #2374, .F. ) ;
#3784 = EDGE_CURVE ( 'NONE', #553, #5560, #5657, .T. ) ;
#3785 = EDGE_CURVE ( 'NONE', #2328, #5405, #6001, .T. ) ;
#3786 = CARTESIAN_POINT ( 'NONE',  ( 0.000000000000000000, 0.000000000000000000, 0.000000000000000000 ) ) ;
#3787 = DIRECTION ( 'NONE',  ( -0.9147661038495519259, 0.4039838799357109989, 3.942553354492744024E-16 ) ) ;
#3788 = DIRECTION ( 'NONE',  ( -0.2467992669038191755, 0.02032136184815236737, 0.9688535307818070264 ) ) ;
#3789 = CARTESIAN_POINT ( 'NONE',  ( -28.68093632328457332, 11.79168739492758711, -1.499999999999988676 ) ) ;
#3790 = CARTESIAN_POINT ( 'NONE',  ( -6.599700898649300207, -61.96243991103532522, 3.420662994399620072 ) ) ;
#3791 = EDGE_LOOP ( 'NONE', ( #218, #3136, #4884, #6213, #7408 ) ) ;
#3792 = ADVANCED_FACE ( 'NONE', ( #4262 ), #3829, .F. ) ;
#3793 = EDGE_CURVE ( 'NONE', #232, #5405, #3533, .T. ) ;
#3794 = CARTESIAN_POINT ( 'NONE',  ( 41.70778007397900211, -94.98992620957551480, -9.454242944073598665E-14 ) ) ;
#3795 = CARTESIAN_POINT ( 'NONE',  ( -1.974098099753330171, -66.57628266072889289, 3.196874607719439876 ) ) ;
#3796 = DIRECTION ( 'NONE',  ( -9.251858538542970644E-15, -2.775557561562891351E-14, -1.000000000000000000 ) ) ;
#3797 = CARTESIAN_POINT ( 'NONE',  ( -19.94212619460463287, -40.63668738334721553, -3.001000000000041634 ) ) ;
#3798 = ORIENTED_EDGE ( 'NONE', *, *, #6426, .T. ) ;
#3799 = EDGE_CURVE ( 'NONE', #5544, #5081, #860, .T. ) ;
#3800 = FACE_OUTER_BOUND ( 'NONE', #6044, .T. ) ;
#3801 = CARTESIAN_POINT ( 'NONE',  ( 3.603225912324908187, 20.45020204625077298, -3.299999999999978950 ) ) ;
#3802 = FACE_OUTER_BOUND ( 'NONE', #7058, .T. ) ;
#3803 = DIRECTION ( 'NONE',  ( -1.602374898470634869E-16, 1.442524254523139935E-17, 1.000000000000000000 ) ) ;
#3804 = DIRECTION ( 'NONE',  ( -0.9999836672264332815, 0.005715354789860036498, 0.000000000000000000 ) ) ;
#3805 = CARTESIAN_POINT ( 'NONE',  ( 6.472013764049630247, -56.98767972836586182, 1.711274884184114775 ) ) ;
#3806 = CARTESIAN_POINT ( 'NONE',  ( -17.18648583462957902, 1.679248046991888677, -3.299999999999998046 ) ) ;
#3807 = ORIENTED_EDGE ( 'NONE', *, *, #6211, .T. ) ;
#3808 = CARTESIAN_POINT ( 'NONE',  ( -19.59526946576633222, 14.55287597139389888, 0.006154456448479242447 ) ) ;
#3809 = CARTESIAN_POINT ( 'NONE',  ( -14.19935799777262453, 13.52206207932379023, 0.4789135844464635361 ) ) ;
#3810 = FACE_OUTER_BOUND ( 'NONE', #5861, .T. ) ;
#3811 = CARTESIAN_POINT ( 'NONE',  ( -2.708443266796834781, -56.15294253968003346, -1.503436295530243827 ) ) ;
#3812 = CYLINDRICAL_SURFACE ( 'NONE', #7003, 1.100000000000000755 ) ;
#3813 = CARTESIAN_POINT ( 'NONE',  ( 4.114990506629828459, -65.14581218975672527, 2.850248089031072407 ) ) ;
#3814 = EDGE_LOOP ( 'NONE', ( #5910, #1101, #6448, #1596 ) ) ;
#3815 = VERTEX_POINT ( 'NONE', #1395 ) ;
#3816 = VERTEX_POINT ( 'NONE', #2061 ) ;
#3817 = CARTESIAN_POINT ( 'NONE',  ( -0.1338713252498902051, -0.05123603448566049767, -7.559811056660412851E-16 ) ) ;
#3818 = CARTESIAN_POINT ( 'NONE',  ( -19.02833027023232404, 14.48681530925147776, 0.1446440811472397281 ) ) ;
#3819 = DIRECTION ( 'NONE',  ( 2.207673464680433438E-16, -2.241093068000311301E-16, 1.000000000000000000 ) ) ;
#3820 = CARTESIAN_POINT ( 'NONE',  ( -95.86211798318534250, -102.0316339954322018, -1.000000000000102807 ) ) ;
#3821 = CARTESIAN_POINT ( 'NONE',  ( 6.187144687173720570, -58.64655194120005177, 0.3691021985165400809 ) ) ;
#3822 = EDGE_CURVE ( 'NONE', #5827, #4944, #2869, .T. ) ;
#3823 = ORIENTED_EDGE ( 'NONE', *, *, #4402, .T. ) ;
#3824 = ORIENTED_EDGE ( 'NONE', *, *, #3734, .F. ) ;
#3825 = CARTESIAN_POINT ( 'NONE',  ( 27.25760507213267658, -34.47413764220541310, -0.2615252949604586208 ) ) ;
#3826 = CARTESIAN_POINT ( 'NONE',  ( -15.08175531864075047, -33.26559167236155190, -4.352666404962730162 ) ) ;
#3827 = CARTESIAN_POINT ( 'NONE',  ( -6.097705871868670080, -61.85866295707492668, 3.539665806518350610 ) ) ;
#3828 = CIRCLE ( 'NONE', #595, 2.999999999999999556 ) ;
#3829 = CYLINDRICAL_SURFACE ( 'NONE', #6138, 140.0000000000000000 ) ;
#3830 = ADVANCED_FACE ( 'NONE', ( #5431 ), #266, .T. ) ;
#3831 = EDGE_CURVE ( 'NONE', #7163, #3179, #2021, .T. ) ;
#3832 = CARTESIAN_POINT ( 'NONE',  ( -6.643389330756649613, -62.64438243220202196, 2.533637634891150459 ) ) ;
#3833 = ORIENTED_EDGE ( 'NONE', *, *, #633, .T. ) ;
#3834 = AXIS2_PLACEMENT_3D ( 'NONE', #6851, #6732, #498 ) ;
#3835 = DIRECTION ( 'NONE',  ( 0.3144066910790611624, 0.9492883822130743221, 0.000000000000000000 ) ) ;
#3836 = B_SPLINE_CURVE_WITH_KNOTS ( 'NONE', 3,
 ( #639, #79, #6958, #1653, #1138, #4563 ),
 .UNSPECIFIED., .F., .F.,
 ( 4, 2, 4 ),
 ( 0.000000000000000000, 0.5000000000000000000, 1.000000000000000000 ),
 .UNSPECIFIED. ) ;
#3837 = LINE ( 'NONE', #6195, #5347 ) ;
#3838 = EDGE_CURVE ( 'NONE', #4842, #2728, #2022, .T. ) ;
#3839 = CARTESIAN_POINT ( 'NONE',  ( 4.860610968486169803, 1.172374092613760688, -3.000000000000000000 ) ) ;
#3840 = AXIS2_PLACEMENT_3D ( 'NONE', #2074, #983, #5597 ) ;
#3841 = CARTESIAN_POINT ( 'NONE',  ( 3.914764119449064772, -54.23824460091720567, 1.533423736523834346 ) ) ;
#3842 = DIRECTION ( 'NONE',  ( -7.159176919053500386E-18, -9.973300763855708376E-16, 1.000000000000000000 ) ) ;
#3843 = EDGE_LOOP ( 'NONE', ( #5160, #173, #7398, #3751 ) ) ;
#3844 = LINE ( 'NONE', #5024, #3736 ) ;
#3845 = CARTESIAN_POINT ( 'NONE',  ( 35.25551690214635414, 7.283442040853450372, -2.999999999999993339 ) ) ;
#3846 = CARTESIAN_POINT ( 'NONE',  ( 8.411763394295572738, 16.69999280642484507, 3.000000000000017764 ) ) ;
#3847 = EDGE_CURVE ( 'NONE', #6538, #418, #3828, .T. ) ;
#3848 = CARTESIAN_POINT ( 'NONE',  ( 1.475197934039484071, -55.33068667649028782, 1.900472455802885818 ) ) ;
#3849 = DIRECTION ( 'NONE',  ( -5.715354789860003484E-18, -9.999836672264337477E-16, 1.000000000000000000 ) ) ;
#3850 = DIRECTION ( 'NONE',  ( -0.9721221936972339606, -0.2344748185227520099, 0.000000000000000000 ) ) ;
#3851 = ORIENTED_EDGE ( 'NONE', *, *, #2406, .F. ) ;
#3852 = CARTESIAN_POINT ( 'NONE',  ( 1.985288149635364929, -66.63130641047898450, -3.284835754603986580 ) ) ;
#3853 = ORIENTED_EDGE ( 'NONE', *, *, #4264, .T. ) ;
#3854 = ORIENTED_EDGE ( 'NONE', *, *, #6239, .F. ) ;
#3855 = DIRECTION ( 'NONE',  ( 1.000000000000000000, 0.000000000000000000, 0.000000000000000000 ) ) ;
#3856 = DIRECTION ( 'NONE',  ( -5.715354789845005112E-18, -9.999836672264339449E-16, 1.000000000000000000 ) ) ;
#3857 = AXIS2_PLACEMENT_3D ( 'NONE', #6421, #4659, #5180 ) ;
#3858 =( LENGTH_UNIT ( ) NAMED_UNIT ( * ) SI_UNIT ( .MILLI., .METRE. ) );
#3859 = FACE_OUTER_BOUND ( 'NONE', #3449, .T. ) ;
#3860 = CARTESIAN_POINT ( 'NONE',  ( 6.751207790105429929, -62.61097121624884210, 0.9581327554396804613 ) ) ;
#3861 = ORIENTED_EDGE ( 'NONE', *, *, #6081, .F. ) ;
#3862 = AXIS2_PLACEMENT_3D ( 'NONE', #5862, #6823, #6271 ) ;
#3863 = DIRECTION ( 'NONE',  ( -0.9999836672264335036, 0.005715354789845008589, 0.000000000000000000 ) ) ;
#3864 = EDGE_CURVE ( 'NONE', #7182, #2474, #1553, .T. ) ;
#3865 = DIRECTION ( 'NONE',  ( -0.5308961072311346729, -0.8474369140690223290, -8.504573326831746910E-16 ) ) ;
#3866 = CARTESIAN_POINT ( 'NONE',  ( 3.660823140336725068, -65.74644859602665292, -1.309095517728299907 ) ) ;
#3867 = VECTOR ( 'NONE', #3639, 1000.000000000000000 ) ;
#3868 = CYLINDRICAL_SURFACE ( 'NONE', #4936, 0.4999999999999978906 ) ;
#3869 = DIRECTION ( 'NONE',  ( 5.715354789845005112E-18, 9.999836672264339449E-16, -1.000000000000000000 ) ) ;
#3870 = AXIS2_PLACEMENT_3D ( 'NONE', #5132, #4600, #6255 ) ;
#3871 = VERTEX_POINT ( 'NONE', #5549 ) ;
#3872 = CIRCLE ( 'NONE', #640, 2.249999999999996891 ) ;
#3873 = CIRCLE ( 'NONE', #5705, 2.250000000000031974 ) ;
#3874 = ADVANCED_FACE ( 'NONE', ( #5588 ), #340, .T. ) ;
#3875 = ADVANCED_FACE ( 'NONE', ( #425 ), #6118, .T. ) ;
#3876 = CARTESIAN_POINT ( 'NONE',  ( 17.61082880304171994, -39.97043410412675968, 2.999999999999957812 ) ) ;
#3877 = CARTESIAN_POINT ( 'NONE',  ( -19.52657036150868208, 8.623428025244434636, -2.230393353321900918 ) ) ;
#3878 = CIRCLE ( 'NONE', #646, 0.7499999999999994449 ) ;
#3879 = CARTESIAN_POINT ( 'NONE',  ( 0.000000000000000000, 0.000000000000000000, 2.544444444444450060 ) ) ;
#3880 = AXIS2_PLACEMENT_3D ( 'NONE', #4993, #2004, #1486 ) ;
#3881 = B_SPLINE_CURVE_WITH_KNOTS ( 'NONE', 3,
 ( #2931, #2479, #4782, #3599 ),
 .UNSPECIFIED., .F., .F.,
 ( 4, 4 ),
 ( 0.000000000000000000, 1.000000000000000000 ),
 .UNSPECIFIED. ) ;
#3882 = CARTESIAN_POINT ( 'NONE',  ( 6.378760423371060639, -64.06988568591069111, -0.05691440262071967293 ) ) ;
#3883 = DIRECTION ( 'NONE',  ( 0.000000000000000000, -1.000000000000000000, -8.673617379884027583E-16 ) ) ;
#3884 = AXIS2_PLACEMENT_3D ( 'NONE', #4503, #3242, #985 ) ;
#3885 = AXIS2_PLACEMENT_3D ( 'NONE', #6335, #740, #4750 ) ;
#3886 = ORIENTED_EDGE ( 'NONE', *, *, #4532, .T. ) ;
#3887 = CARTESIAN_POINT ( 'NONE',  ( -12.68640736393857082, 13.22347097710891717, 1.616354215094460922E-14 ) ) ;
#3888 = ADVANCED_FACE ( 'NONE', ( #4978 ), #6151, .T. ) ;
#3889 = CARTESIAN_POINT ( 'NONE',  ( -4.957894848432390589, -59.36360895465049481, -1.768545648133530879 ) ) ;
#3890 = DIRECTION ( 'NONE',  ( 0.4039838799357100552, 0.9147661038495522590, 4.432239818696549050E-17 ) ) ;
#3891 = VECTOR ( 'NONE', #5097, 1000.000000000000000 ) ;
#3892 = DIRECTION ( 'NONE',  ( -0.9828140593167949968, 0.1845982795403122156, 4.010227384219995304E-16 ) ) ;
#3893 = CARTESIAN_POINT ( 'NONE',  ( -4.930053471857299918, -61.64676491032937378, 0.1765652348176402209 ) ) ;
#3894 = CARTESIAN_POINT ( 'NONE',  ( 27.29354050645795482, -34.45366325832522136, 3.130828461196526469 ) ) ;
#3895 = DIRECTION ( 'NONE',  ( -5.715354789845005112E-18, -9.999836672264339449E-16, 1.000000000000000000 ) ) ;
#3896 = VECTOR ( 'NONE', #1934, 1000.000000000000000 ) ;
#3897 = ORIENTED_EDGE ( 'NONE', *, *, #2035, .T. ) ;
#3898 = ORIENTED_EDGE ( 'NONE', *, *, #1540, .F. ) ;
#3899 = ADVANCED_FACE ( 'NONE', ( #3348 ), #234, .T. ) ;
#3900 = DIRECTION ( 'NONE',  ( 0.9999836672264332815, -0.005715354789845306094, 0.000000000000000000 ) ) ;
#3901 = EDGE_LOOP ( 'NONE', ( #3116, #1872, #4776, #5552, #2756, #2093 ) ) ;
#3902 =( NAMED_UNIT ( * ) PLANE_ANGLE_UNIT ( ) SI_UNIT ( $, .RADIAN. ) );
#3903 = CARTESIAN_POINT ( 'NONE',  ( -45.28625779897078729, -94.36209361619114588, -9.461937945190903839E-14 ) ) ;
#3904 = FACE_BOUND ( 'NONE', #4666, .T. ) ;
#3905 = CARTESIAN_POINT ( 'NONE',  ( 6.443572816261259995, -63.55558822192794111, -2.176462561484786118 ) ) ;
#3906 = EDGE_LOOP ( 'NONE', ( #3506, #7400, #4205, #6711 ) ) ;
#3907 = ORIENTED_EDGE ( 'NONE', *, *, #4602, .F. ) ;
#3908 = LINE ( 'NONE', #3305, #1346 ) ;
#3909 = CARTESIAN_POINT ( 'NONE',  ( -5.563801105733269914, -63.69014839564722763, 1.341242183458755344 ) ) ;
#3910 = ORIENTED_EDGE ( 'NONE', *, *, #4724, .F. ) ;
#3911 = PLANE ( 'NONE',  #3834 ) ;
#3912 =( BOUNDED_SURFACE ( )  B_SPLINE_SURFACE ( 3, 2, ( 
 ( #72, #5764, #1727 ),
 ( #5163, #4026, #2283 ),
 ( #4134, #4672, #2921 ),
 ( #2989, #4703, #1168 ),
 ( #3452, #3485, #1798 ),
 ( #5273, #2393, #5804 ),
 ( #592, #30, #631 ),
 ( #2326, #5240, #2363 ),
 ( #6954, #7031, #6435 ),
 ( #1283, #3562, #136 ) ),
 .UNSPECIFIED., .F., .F., .T. ) 
 B_SPLINE_SURFACE_WITH_KNOTS ( ( 4, 2, 2, 2, 4 ),
 ( 3, 3 ),
 ( 0.000000000000000000, 0.0001952887240141836802, 0.0003905774480283673604, 0.0005858661720425509863, 0.0007811548960567347207 ),
 ( 0.000000000000000000, 1.000000000000000000 ),
 .UNSPECIFIED. ) 
 GEOMETRIC_REPRESENTATION_ITEM ( )  RATIONAL_B_SPLINE_SURFACE ( (
 ( 1.000000000000000000, 0.7071067811865472397, 1.000000000000000000),
 ( 1.000000000000000000, 0.7061982418737673406, 1.000000000000000000),
 ( 1.000000000000000000, 0.7052889306346207254, 1.000000000000000000),
 ( 1.000000000000000000, 0.7036054371094994098, 1.000000000000000000),
 ( 1.000000000000000000, 0.7028338995551517421, 1.000000000000000000),
 ( 1.000000000000000000, 0.7015497601672633365, 1.000000000000000000),
 ( 1.000000000000000000, 0.7010307650890416076, 1.000000000000000000),
 ( 1.000000000000000000, 0.7003352509067762854, 1.000000000000000000),
 ( 1.000000000000000000, 0.7001488311338350812, 1.000000000000000000),
 ( 1.000000000000000000, 0.7001503461741274137, 1.000000000000000000) ) ) 
 REPRESENTATION_ITEM ( '' )  SURFACE ( )  );
#3913 = CARTESIAN_POINT ( 'NONE',  ( 11.37011796090756555, -1.723489934710175753, -1.734723475976807094E-15 ) ) ;
#3914 = ORIENTED_EDGE ( 'NONE', *, *, #6706, .F. ) ;
#3915 = EDGE_CURVE ( 'NONE', #3496, #1942, #719, .T. ) ;
#3916 = ORIENTED_EDGE ( 'NONE', *, *, #7022, .F. ) ;
#3917 = CARTESIAN_POINT ( 'NONE',  ( 17.88843813672056626, -40.41242482140539494, 2.999999999999957367 ) ) ;
#3918 = DIRECTION ( 'NONE',  ( -0.9858503002877112564, 0.1676281164441980331, 1.619908943762944784E-16 ) ) ;
#3919 = CARTESIAN_POINT ( 'NONE',  ( 31.14423615379030608, -4.720863734206126594, -4.336808689942017736E-15 ) ) ;
#3920 = CARTESIAN_POINT ( 'NONE',  ( -6.240992105565960735, -57.07993508854151798, -2.135104940435555765 ) ) ;
#3921 = LINE ( 'NONE', #5144, #649 ) ;
#3922 = VERTEX_POINT ( 'NONE', #5049 ) ;
#3923 = DIRECTION ( 'NONE',  ( 0.9999836672264332815, -0.005715354789847320975, 0.000000000000000000 ) ) ;
#3924 = CARTESIAN_POINT ( 'NONE',  ( 4.922451174039159660, -61.67826628571419434, -0.7081498598146799273 ) ) ;
#3925 = LINE ( 'NONE', #2190, #1610 ) ;
#3926 = CARTESIAN_POINT ( 'NONE',  ( 10.26069562290071957, -51.72814510619807749, -2.502481404895003259 ) ) ;
#3927 = CARTESIAN_POINT ( 'NONE',  ( -4.302337887170949671, -63.34626699285441020, 3.181678273100430054 ) ) ;
#3928 = CARTESIAN_POINT ( 'NONE',  ( 26.87031364676134970, -34.69479876584121314, 3.499999999999965805 ) ) ;
#3929 = EDGE_CURVE ( 'NONE', #3331, #1468, #601, .T. ) ;
#3930 = CARTESIAN_POINT ( 'NONE',  ( -33.11453295935376673, 14.62421645367269463, 1.431146867680865853E-14 ) ) ;
#3931 = ORIENTED_EDGE ( 'NONE', *, *, #803, .F. ) ;
#3932 = EDGE_CURVE ( 'NONE', #5578, #7182, #4082, .T. ) ;
#3933 = CARTESIAN_POINT ( 'NONE',  ( -3.018293710664720297, -66.19764165108277609, -3.019563749174228207 ) ) ;
#3934 = VERTEX_POINT ( 'NONE', #4488 ) ;
#3935 = ORIENTED_EDGE ( 'NONE', *, *, #7033, .F. ) ;
#3936 = ORIENTED_EDGE ( 'NONE', *, *, #3929, .F. ) ;
#3937 = CARTESIAN_POINT ( 'NONE',  ( -15.07233531785332659, 13.90759097395377886, 2.236547809770392803 ) ) ;
#3938 = VERTEX_POINT ( 'NONE', #2292 ) ;
#3939 = B_SPLINE_CURVE_WITH_KNOTS ( 'NONE', 3,
 ( #5751, #4832, #5863, #4691, #4158, #5368 ),
 .UNSPECIFIED., .F., .F.,
 ( 4, 2, 4 ),
 ( 0.000000000000000000, 0.0003937726336352555625, 0.0007875452672705111250 ),
 .UNSPECIFIED. ) ;
#3940 = CYLINDRICAL_SURFACE ( 'NONE', #1482, 3.750000000000000444 ) ;
#3941 = DIRECTION ( 'NONE',  ( -0.2344748185227520099, 0.9721221936972339606, 0.000000000000000000 ) ) ;
#3942 = CARTESIAN_POINT ( 'NONE',  ( 2.066956868921485224, -53.66058936408188629, 0.4281972772843347652 ) ) ;
#3943 = ORIENTED_EDGE ( 'NONE', *, *, #38, .F. ) ;
#3944 = ADVANCED_FACE ( 'NONE', ( #6188 ), #4529, .T. ) ;
#3945 =( REPRESENTATION_RELATIONSHIP ('NONE','NONE', #3195, #4460 ) REPRESENTATION_RELATIONSHIP_WITH_TRANSFORMATION ( #5682 )SHAPE_REPRESENTATION_RELATIONSHIP( ) );
#3946 = VERTEX_POINT ( 'NONE', #6225 ) ;
#3947 = DIRECTION ( 'NONE',  ( 0.3144019573014844582, -0.9492899500389728740, 0.000000000000000000 ) ) ;
#3948 = DIRECTION ( 'NONE',  ( 0.6513146796332660582, 0.5900073775824583588, -0.4771587602596085165 ) ) ;
#3949 = DIRECTION ( 'NONE',  ( -1.602374898470634869E-16, 1.442524254523139935E-17, 1.000000000000000000 ) ) ;
#3950 = CARTESIAN_POINT ( 'NONE',  ( 14.81352433457121975, -34.80119172639020064, 0.4975185951050001831 ) ) ;
#3951 = CARTESIAN_POINT ( 'NONE',  ( 4.860610968486169803, 1.172374092613760688, -17.67054229618195293 ) ) ;
#3952 = CARTESIAN_POINT ( 'NONE',  ( 104.0973215944787711, -119.5240462704291389, -3.000000000000119904 ) ) ;
#3953 = EDGE_LOOP ( 'NONE', ( #5337, #2872, #3311, #208 ) ) ;
#3954 = CARTESIAN_POINT ( 'NONE',  ( 1.714606436953501688E-17, 2.999951001679301835E-15, 0.000000000000000000 ) ) ;
#3955 = DIRECTION ( 'NONE',  ( -3.426943000455268076E-15, 1.019602848034623186E-15, -1.000000000000000000 ) ) ;
#3956 = CARTESIAN_POINT ( 'NONE',  ( -4.418648243523263019, 30.02574454609010601, 2.992397996059992238E-14 ) ) ;
#3957 = CARTESIAN_POINT ( 'NONE',  ( 3.751014749966880224, -66.74975575182239140, 0.1208598729073953049 ) ) ;
#3958 = CARTESIAN_POINT ( 'NONE',  ( 14.63763862841553376, 20.11382921380832656, -1.993845543551509447 ) ) ;
#3959 = AXIS2_PLACEMENT_3D ( 'NONE', #145, #1807, #680 ) ;
#3960 = ORIENTED_EDGE ( 'NONE', *, *, #2769, .F. ) ;
#3961 = CARTESIAN_POINT ( 'NONE',  ( -21.54648976118723525, 4.049597505996694657, -2.230393353321905359 ) ) ;
#3962 = CARTESIAN_POINT ( 'NONE',  ( 4.890810490072590611, -59.09042288871975757, -0.8837144134564199893 ) ) ;
#3963 = EDGE_CURVE ( 'NONE', #5506, #320, #2025, .T. ) ;
#3964 = DIRECTION ( 'NONE',  ( 0.8856191127862077517, 0.4644123028815776988, 4.694663451788343547E-16 ) ) ;
#3965 = VECTOR ( 'NONE', #6735, 1000.000000000000000 ) ;
#3966 = DIRECTION ( 'NONE',  ( 0.9492899500389727629, 0.3144019573014849023, 0.000000000000000000 ) ) ;
#3967 = CARTESIAN_POINT ( 'NONE',  ( 5.090297305459900556, -61.99464686763499088, 2.430409751936420282 ) ) ;
#3968 = DIRECTION ( 'NONE',  ( 0.000000000000000000, -0.7252570966694443788, 0.6884781359858918037 ) ) ;
#3969 = DIRECTION ( 'NONE',  ( 0.9999836672264335036, -0.005715354789845041548, 0.000000000000000000 ) ) ;
#3970 = VERTEX_POINT ( 'NONE', #2852 ) ;
#3971 = ORIENTED_EDGE ( 'NONE', *, *, #2036, .F. ) ;
#3972 = ORIENTED_EDGE ( 'NONE', *, *, #4687, .F. ) ;
#3973 = AXIS2_PLACEMENT_3D ( 'NONE', #2420, #5868, #7055 ) ;
#3974 = EDGE_CURVE ( 'NONE', #6398, #5434, #6402, .T. ) ;
#3975 = EDGE_CURVE ( 'NONE', #1643, #5210, #2171, .T. ) ;
#3976 = CARTESIAN_POINT ( 'NONE',  ( 39.48483786921892857, -95.33781693134928048, -9.497611030973018842E-14 ) ) ;
#3977 = ORIENTED_EDGE ( 'NONE', *, *, #971, .T. ) ;
#3978 = LINE ( 'NONE', #2361, #4002 ) ;
#3979 = DIRECTION ( 'NONE',  ( -0.6713653717953944611, 0.7411265327553937521, 3.821372782371133360E-16 ) ) ;
#3980 = AXIS2_PLACEMENT_3D ( 'NONE', #3125, #6527, #279 ) ;
#3981 = CARTESIAN_POINT ( 'NONE',  ( -105.7473861751082040, -118.0666774205683822, -1.188285581044112860E-13 ) ) ;
#3982 = CARTESIAN_POINT ( 'NONE',  ( -6.238287558858839787, -63.42668406018486849, 1.752565146537014895 ) ) ;
#3983 = EDGE_LOOP ( 'NONE', ( #5017, #6844, #7174 ) ) ;
#3984 = DIRECTION ( 'NONE',  ( 0.9999836672264332815, -0.005715354789859975783, 0.000000000000000000 ) ) ;
#3985 = VECTOR ( 'NONE', #3205, 1000.000000000000114 ) ;
#3986 = CYLINDRICAL_SURFACE ( 'NONE', #4618, 2.249999999999996891 ) ;
#3987 = EDGE_CURVE ( 'NONE', #4283, #4962, #6260, .T. ) ;
#3988 = DIRECTION ( 'NONE',  ( 0.6713653717953971256, -0.7411265327553914206, -7.372773368101212272E-16 ) ) ;
#3989 = DIRECTION ( 'NONE',  ( -0.3144019573014849023, 0.9492899500389726519, 0.000000000000000000 ) ) ;
#3990 = FACE_OUTER_BOUND ( 'NONE', #2741, .T. ) ;
#3991 = FACE_OUTER_BOUND ( 'NONE', #6497, .T. ) ;
#3992 = CIRCLE ( 'NONE', #1582, 0.7500000000000000000 ) ;
#3993 = ORIENTED_EDGE ( 'NONE', *, *, #1589, .T. ) ;
#3994 = VECTOR ( 'NONE', #6511, 1000.000000000000000 ) ;
#3995 = AXIS2_PLACEMENT_3D ( 'NONE', #1017, #2770, #2735 ) ;
#3996 = CARTESIAN_POINT ( 'NONE',  ( 17.72543015532271937, -39.90513944096638710, 3.513721684389295330 ) ) ;
#3997 = CIRCLE ( 'NONE', #5933, 2.499999999999996891 ) ;
#3998 = DIRECTION ( 'NONE',  ( 0.4039838799357088894, 0.9147661038495528141, -4.517316048718991978E-16 ) ) ;
#3999 = LINE ( 'NONE', #6310, #6731 ) ;
#4000 = CARTESIAN_POINT ( 'NONE',  ( 6.281284389406939894, -57.15453665621128465, 0.6930907858711948810 ) ) ;
#4001 = CARTESIAN_POINT ( 'NONE',  ( 30.52077159997833533, 5.488396937353885896, -1.499999999999994893 ) ) ;
#4002 = VECTOR ( 'NONE', #5845, 1000.000000000000114 ) ;
#4003 = CIRCLE ( 'NONE', #3265, 1.000000000000000000 ) ;
#4004 = ORIENTED_EDGE ( 'NONE', *, *, #2444, .F. ) ;
#4005 = CARTESIAN_POINT ( 'NONE',  ( 17.88843813672054850, -40.41242482140538073, 3.264142021185714171 ) ) ;
#4006 = CARTESIAN_POINT ( 'NONE',  ( -24.22739558392570203, 5.420192826457481239, 3.306154456448477497 ) ) ;
#4007 = AXIS2_PLACEMENT_3D ( 'NONE', #3511, #5225, #61 ) ;
#4008 = AXIS2_PLACEMENT_3D ( 'NONE', #2877, #2841, #2804 ) ;
#4009 = DIRECTION ( 'NONE',  ( -0.9147661038495517039, 0.4039838799357113874, -4.956352788505161098E-15 ) ) ;
#4010 = CARTESIAN_POINT ( 'NONE',  ( 5.175864525269250116, -61.68163375030346174, 0.3100344153189201202 ) ) ;
#4011 = AXIS2_PLACEMENT_3D ( 'NONE', #2141, #2181, #1591 ) ;
#4012 = AXIS2_PLACEMENT_3D ( 'NONE', #1389, #7071, #223 ) ;
#4013 = CARTESIAN_POINT ( 'NONE',  ( 27.24996190780300509, -34.47849237127667266, 3.251881639501436272 ) ) ;
#4014 = DIRECTION ( 'NONE',  ( -0.4039838799357104993, -0.9147661038495521479, -9.170600743851227050E-16 ) ) ;
#4015 = ORIENTED_EDGE ( 'NONE', *, *, #4707, .T. ) ;
#4016 = ORIENTED_EDGE ( 'NONE', *, *, #3219, .F. ) ;
#4017 = ADVANCED_FACE ( 'NONE', ( #4565 ), #3911, .F. ) ;
#4018 = ORIENTED_EDGE ( 'NONE', *, *, #707, .T. ) ;
#4019 = ORIENTED_EDGE ( 'NONE', *, *, #7011, .T. ) ;
#4020 = AXIS2_PLACEMENT_3D ( 'NONE', #387, #3594, #4387 ) ;
#4021 = ITEM_DEFINED_TRANSFORMATION ( 'NONE', 'NONE', #6305,  #751 ) ;
#4022 = DIRECTION ( 'NONE',  ( 0.3144066910790611624, 0.9492883822130743221, 0.000000000000000000 ) ) ;
#4023 = VERTEX_POINT ( 'NONE', #7334 ) ;
#4024 = PLANE ( 'NONE',  #3028 ) ;
#4025 = FACE_BOUND ( 'NONE', #5561, .T. ) ;
#4026 = CARTESIAN_POINT ( 'NONE',  ( 26.98408672118752349, -34.62997601791116153, -1.001286369213168825 ) ) ;
#4027 = CARTESIAN_POINT ( 'NONE',  ( -1.862703854971429873, -67.54117654042293850, 0.3860096597272351659 ) ) ;
#4028 = ORIENTED_EDGE ( 'NONE', *, *, #3793, .T. ) ;
#4029 = VERTEX_POINT ( 'NONE', #6894 ) ;
#4030 = ADVANCED_FACE ( 'NONE', ( #3990 ), #3868, .T. ) ;
#4031 = ORIENTED_EDGE ( 'NONE', *, *, #1343, .T. ) ;
#4032 = SURFACE_SIDE_STYLE ('',( #7370 ) ) ;
#4033 = LINE ( 'NONE', #2884, #4368 ) ;
#4034 = FACE_OUTER_BOUND ( 'NONE', #490, .T. ) ;
#4035 = CARTESIAN_POINT ( 'NONE',  ( 5.564888630279786419, -62.34576501924355796, -3.501689517682560648 ) ) ;
#4036 = CARTESIAN_POINT ( 'NONE',  ( -95.86211798318534250, -102.0316339954322018, 2.999999999999897415 ) ) ;
#4037 =( LENGTH_UNIT ( ) NAMED_UNIT ( * ) SI_UNIT ( .MILLI., .METRE. ) );
#4038 = EDGE_CURVE ( 'NONE', #6025, #6356, #458, .T. ) ;
#4039 = ADVANCED_FACE ( 'NONE', ( #6300 ), #2739, .T. ) ;
#4040 = VERTEX_POINT ( 'NONE', #2820 ) ;
#4041 = CARTESIAN_POINT ( 'NONE',  ( 18.21934571153571980, -40.21434464133486841, 3.799679232396574236 ) ) ;
#4042 = CARTESIAN_POINT ( 'NONE',  ( -9.389556988382800284, -51.17759447638420767, 3.521321650943620707 ) ) ;
#4043 = DIRECTION ( 'NONE',  ( 0.000000000000000000, -0.7252570966694443788, 0.6884781359858918037 ) ) ;
#4044 = CARTESIAN_POINT ( 'NONE',  ( -6.814417183322500016, -58.48210382454914935, -0.1019614231452001113 ) ) ;
#4045 = CARTESIAN_POINT ( 'NONE',  ( 4.492111197601039052, 14.38610368760445546, 1.431146867680865853E-14 ) ) ;
#4046 = ORIENTED_EDGE ( 'NONE', *, *, #5966, .F. ) ;
#4047 = CYLINDRICAL_SURFACE ( 'NONE', #5436, 147.0000000000000000 ) ;
#4048 = SURFACE_SIDE_STYLE ('',( #5181 ) ) ;
#4049 = DIRECTION ( 'NONE',  ( -0.4039838799357098331, -0.9147661038495523700, -8.673617379884154787E-16 ) ) ;
#4050 = CARTESIAN_POINT ( 'NONE',  ( -34.88460058024262622, 16.28046363954885933, -2.243845543551999722 ) ) ;
#4051 = CARTESIAN_POINT ( 'NONE',  ( -5.065438427596520299, -62.07564176717611559, -0.9259012332463799622 ) ) ;
#4052 = CARTESIAN_POINT ( 'NONE',  ( 27.09963614945447219, -34.56414118396787671, 3.975998075095239503 ) ) ;
#4053 = DIRECTION ( 'NONE',  ( 0.9147661038495520369, -0.4039838799357104437, -3.987490689252506674E-16 ) ) ;
#4054 = ORIENTED_EDGE ( 'NONE', *, *, #4346, .F. ) ;
#4055 = ORIENTED_EDGE ( 'NONE', *, *, #5919, .T. ) ;
#4056 = VERTEX_POINT ( 'NONE', #1141 ) ;
#4057 = LINE ( 'NONE', #3370, #6649 ) ;
#4058 = LINE ( 'NONE', #6359, #7365 ) ;
#4059 = CARTESIAN_POINT ( 'NONE',  ( 5.396949887678069935, -64.06165292293543700, 0.6913201402231599069 ) ) ;
#4060 = DIRECTION ( 'NONE',  ( -0.3536350175650657124, -0.3203478684871222115, -0.8788171126619652718 ) ) ;
#4061 = CARTESIAN_POINT ( 'NONE',  ( 4.826828241146579934, -57.92957641372471755, 0.5758163846279100717 ) ) ;
#4062 = ORIENTED_EDGE ( 'NONE', *, *, #3735, .T. ) ;
#4063 = DIRECTION ( 'NONE',  ( -5.715354789845005112E-18, -9.999836672264339449E-16, 1.000000000000000000 ) ) ;
#4064 = DIRECTION ( 'NONE',  ( -0.9492883822130744331, 0.3144066910790611624, 0.000000000000000000 ) ) ;
#4065 = EDGE_CURVE ( 'NONE', #7056, #1273, #3112, .T. ) ;
#4066 = CARTESIAN_POINT ( 'NONE',  ( 26.37580682046979774, 24.48813337504584098, -0.8353469048619511783 ) ) ;
#4067 = FACE_OUTER_BOUND ( 'NONE', #4408, .T. ) ;
#4068 = CARTESIAN_POINT ( 'NONE',  ( 0.000000000000000000, 0.000000000000000000, -3.500000000000000000 ) ) ;
#4069 = CARTESIAN_POINT ( 'NONE',  ( -12.75609440306747189, -34.09959597428994726, -3.417194463855666027E-14 ) ) ;
#4070 = ORIENTED_EDGE ( 'NONE', *, *, #1144, .T. ) ;
#4071 = ORIENTED_EDGE ( 'NONE', *, *, #6599, .F. ) ;
#4072 = EDGE_CURVE ( 'NONE', #4319, #3871, #6471, .T. ) ;
#4073 = EDGE_CURVE ( 'NONE', #1170, #6097, #3481, .T. ) ;
#4074 = DIRECTION ( 'NONE',  ( 0.05111947575940102573, -0.9986925448795961335, 1.285697817222219874E-14 ) ) ;
#4075 = DIRECTION ( 'NONE',  ( 0.03652191451860400950, 0.9993328523369456873, 9.995252661588299226E-16 ) ) ;
#4076 = ORIENTED_EDGE ( 'NONE', *, *, #6582, .F. ) ;
#4077 = CARTESIAN_POINT ( 'NONE',  ( 17.88843813672055916, -40.41242482140538783, 2.999999999999959588 ) ) ;
#4078 = SURFACE_STYLE_USAGE ( .BOTH. , #4048 ) ;
#4079 = EDGE_CURVE ( 'NONE', #3333, #6558, #6727, .T. ) ;
#4080 = CARTESIAN_POINT ( 'NONE',  ( 28.22862315235815345, 26.16654680453439852, -0.8353469048621777748 ) ) ;
#4081 = CARTESIAN_POINT ( 'NONE',  ( -1.747150726250749964, -54.79256248330700174, -0.04158717877314997702 ) ) ;
#4082 = CIRCLE ( 'NONE', #1677, 147.0000000000000284 ) ;
#4083 = CARTESIAN_POINT ( 'NONE',  ( 3.059030343303239974, -54.77303090793805040, 0.1039292770420399137 ) ) ;
#4084 = LINE ( 'NONE', #4164, #7222 ) ;
#4085 = ORIENTED_EDGE ( 'NONE', *, *, #439, .T. ) ;
#4086 = EDGE_LOOP ( 'NONE', ( #3897, #4479, #4400, #6121, #2534, #1971 ) ) ;
#4087 = ORIENTED_EDGE ( 'NONE', *, *, #381, .T. ) ;
#4088 = AXIS2_PLACEMENT_3D ( 'NONE', #1177, #5658, #5135 ) ;
#4089 = CARTESIAN_POINT ( 'NONE',  ( -16.40387102536037744, 1.778486824056636939, 3.000000000000001776 ) ) ;
#4090 = DIRECTION ( 'NONE',  ( -0.5941197849118597940, -0.8043765792067080200, -8.077590468646243185E-16 ) ) ;
#4091 = CARTESIAN_POINT ( 'NONE',  ( -5.982481740117790103, -62.36145600051965232, 1.442409191505919619 ) ) ;
#4092 = CARTESIAN_POINT ( 'NONE',  ( 15.02372294165784794, -37.34713278632150235, -0.9950371902099899302 ) ) ;
#4093 = EDGE_LOOP ( 'NONE', ( #3772, #2119, #5570, #2158 ) ) ;
#4094 = AXIS2_PLACEMENT_3D ( 'NONE', #5288, #4612, #4571 ) ;
#4095 = ORIENTED_EDGE ( 'NONE', *, *, #198, .T. ) ;
#4096 =( NAMED_UNIT ( * ) SI_UNIT ( $, .STERADIAN. ) SOLID_ANGLE_UNIT ( ) );
#4097 = CARTESIAN_POINT ( 'NONE',  ( -14.70408710852078116, -35.66654345889202204, -3.575000000000001175E-14 ) ) ;
#4098 = CIRCLE ( 'NONE', #3373, 20.00000000000000711 ) ;
#4099 = PRODUCT_DEFINITION_SHAPE ( 'NONE', 'NONE',  #7448 ) ;
#4100 = DIRECTION ( 'NONE',  ( -0.6713653717954000122, 0.7411265327553888671, 8.673617379884183383E-16 ) ) ;
#4101 = DIRECTION ( 'NONE',  ( 0.9492899500389727629, 0.3144019573014849023, 0.000000000000000000 ) ) ;
#4102 = CARTESIAN_POINT ( 'NONE',  ( -3.156642594714314853, -54.82761582543010093, 1.871643660998590697 ) ) ;
#4103 = CARTESIAN_POINT ( 'NONE',  ( -45.28625779897078729, -94.36209361619114588, -9.461937945190903839E-14 ) ) ;
#4104 = AXIS2_PLACEMENT_3D ( 'NONE', #4917, #7198, #6632 ) ;
#4105 = ADVANCED_FACE ( 'NONE', ( #1252 ), #42, .F. ) ;
#4106 = CARTESIAN_POINT ( 'NONE',  ( -1.429016193381374089, -55.57463605963037168, -1.413872718151093721 ) ) ;
#4107 = FACE_OUTER_BOUND ( 'NONE', #3814, .T. ) ;
#4108 = DIRECTION ( 'NONE',  ( 0.9999836672264332815, -0.005715354789859956701, 0.000000000000000000 ) ) ;
#4109 = CARTESIAN_POINT ( 'NONE',  ( -3.697637789055789881, -65.78881948023087034, 1.221121406208630411 ) ) ;
#4110 = DIRECTION ( 'NONE',  ( -9.251858538542970644E-15, -2.775557561562891351E-14, -1.000000000000000000 ) ) ;
#4111 = ORIENTED_EDGE ( 'NONE', *, *, #2636, .T. ) ;
#4112 = ADVANCED_FACE ( 'NONE', ( #4649 ), #5964, .T. ) ;
#4113 = EDGE_CURVE ( 'NONE', #1914, #961, #4180, .T. ) ;
#4114 = AXIS2_PLACEMENT_3D ( 'NONE', #6569, #5985, #4843 ) ;
#4115 = CARTESIAN_POINT ( 'NONE',  ( 9.998427761233271482, -32.39925913208585939, 2.999999999999967581 ) ) ;
#4116 = VECTOR ( 'NONE', #3849, 1000.000000000000000 ) ;
#4117 = PRODUCT_DEFINITION ( 'UNKNOWN', '', #6650, #2604 ) ;
#4118 = LINE ( 'NONE', #4189, #4622 ) ;
#4119 = AXIS2_PLACEMENT_3D ( 'NONE', #2891, #1778, #5213 ) ;
#4120 = CARTESIAN_POINT ( 'NONE',  ( 4.638831626566389588, -63.05209213275327329, 0.3994218305236152400 ) ) ;
#4121 = CARTESIAN_POINT ( 'NONE',  ( 5.619938529503549773, -63.59344562873818774, 0.6343307546824898946 ) ) ;
#4122 = FACE_OUTER_BOUND ( 'NONE', #6873, .T. ) ;
#4123 = COLOUR_RGB ( '', 0.72549020, 0.75294118, 0.79215686) ;
#4124 = EDGE_CURVE ( 'NONE', #2474, #3729, #741, .T. ) ;
#4125 = EDGE_CURVE ( 'NONE', #74, #2280, #6145, .T. ) ;
#4126 = ORIENTED_EDGE ( 'NONE', *, *, #1053, .F. ) ;
#4127 = ORIENTED_EDGE ( 'NONE', *, *, #3082, .F. ) ;
#4128 = AXIS2_PLACEMENT_3D ( 'NONE', #7090, #7029, #4201 ) ;
#4129 = VECTOR ( 'NONE', #5683, 1000.000000000000000 ) ;
#4130 = DIRECTION ( 'NONE',  ( 5.715354789845005112E-18, 9.999836672264339449E-16, -1.000000000000000000 ) ) ;
#4131 = AXIS2_PLACEMENT_3D ( 'NONE', #7217, #2550, #4213 ) ;
#4132 = DIRECTION ( 'NONE',  ( -0.9147661038495520369, 0.4039838799357109433, 3.987490689252511604E-16 ) ) ;
#4133 = CARTESIAN_POINT ( 'NONE',  ( -6.921793923077749433, -58.90709844370859116, -2.222636374480685184 ) ) ;
#4134 = CARTESIAN_POINT ( 'NONE',  ( 26.98398549905668986, -34.63003368969938123, -0.4870132424029344209 ) ) ;
#4135 = CIRCLE ( 'NONE', #880, 1.000000000000001110 ) ;
#4136 = B_SPLINE_CURVE_WITH_KNOTS ( 'NONE', 3,
 ( #117, #3574, #710, #3000, #2704, #6216 ),
 .UNSPECIFIED., .F., .F.,
 ( 4, 2, 4 ),
 ( 0.000000000000000000, 0.5000000000000000000, 1.000000000000000000 ),
 .UNSPECIFIED. ) ;
#4137 = EDGE_CURVE ( 'NONE', #5210, #2395, #6376, .T. ) ;
#4138 = AXIS2_PLACEMENT_3D ( 'NONE', #576, #5891, #6907 ) ;
#4139 = ORIENTED_EDGE ( 'NONE', *, *, #4125, .T. ) ;
#4140 = AXIS2_PLACEMENT_3D ( 'NONE', #3526, #4060, #5196 ) ;
#4141 = SHAPE_REPRESENTATION_RELATIONSHIP ( 'NONE' , 'NONE' ,  #3150, #2149 ) ;
#4142 = FACE_OUTER_BOUND ( 'NONE', #6541, .T. ) ;
#4143 = CYLINDRICAL_SURFACE ( 'NONE', #656, 6.500000000000001776 ) ;
#4144 = TOROIDAL_SURFACE ( 'NONE', #4987, 1.500000000000000000, 1.000000000000000000 ) ;
#4145 = DIRECTION ( 'NONE',  ( 0.9999836672264332815, -0.005715354789859936752, 0.000000000000000000 ) ) ;
#4146 = DIRECTION ( 'NONE',  ( 0.9999836672264333925, -0.005715354789860572528, 0.000000000000000000 ) ) ;
#4147 = CARTESIAN_POINT ( 'NONE',  ( -0.9369902355999032428, -66.67870154919400250, 1.040922737850055846 ) ) ;
#4148 = ORIENTED_EDGE ( 'NONE', *, *, #3793, .F. ) ;
#4149 = AXIS2_PLACEMENT_3D ( 'NONE', #2662, #2549, #3788 ) ;
#4150 = CARTESIAN_POINT ( 'NONE',  ( -9.311346830843410416, -51.41373841511900622, 1.033728595105000148 ) ) ;
#4151 = SPHERICAL_SURFACE ( 'NONE', #5048, 7.844444444444450326 ) ;
#4152 = EDGE_CURVE ( 'NONE', #6387, #1973, #2278, .T. ) ;
#4153 = DIRECTION ( 'NONE',  ( -0.9979653668924883814, 0.06375834441969779887, 5.805357692931203648E-17 ) ) ;
#4154 = CARTESIAN_POINT ( 'NONE',  ( -3.079777581550224852, -54.72070545288789134, -0.1918259013367045740 ) ) ;
#4155 = DIRECTION ( 'NONE',  ( 0.2223157560262044585, -0.6712493609847989262, 0.7071067811865449082 ) ) ;
#4156 = ORIENTED_EDGE ( 'NONE', *, *, #252, .T. ) ;
#4157 = DIRECTION ( 'NONE',  ( -0.4950421911735689018, 0.8688689365825386091, 0.000000000000000000 ) ) ;
#4158 = CARTESIAN_POINT ( 'NONE',  ( 27.30483170388658820, -34.44723004512044184, 3.132067106505118215 ) ) ;
#4159 = CARTESIAN_POINT ( 'NONE',  ( -17.04733905648494030, -8.234069079964159599, -8.331366185709195643E-15 ) ) ;
#4160 = CARTESIAN_POINT ( 'NONE',  ( 17.95758103425560748, -39.77287037833651340, -0.8100516860784414686 ) ) ;
#4161 = ADVANCED_FACE ( 'NONE', ( #2402 ), #5256, .T. ) ;
#4162 = CARTESIAN_POINT ( 'NONE',  ( 1.570963842414029976, -66.14661321919228953, 1.018783762524700265 ) ) ;
#4163 = DIRECTION ( 'NONE',  ( 0.9999836672264332815, -0.005715354789859936752, 0.000000000000000000 ) ) ;
#4164 = CARTESIAN_POINT ( 'NONE',  ( -33.11453295935376673, 14.62421645367269107, 3.000000000000014211 ) ) ;
#4165 = VERTEX_POINT ( 'NONE', #3725 ) ;
#4166 = VERTEX_POINT ( 'NONE', #4835 ) ;
#4167 = ORIENTED_EDGE ( 'NONE', *, *, #3196, .F. ) ;
#4168 = DIRECTION ( 'NONE',  ( -5.715354789860003484E-18, -9.999836672264337477E-16, 1.000000000000000000 ) ) ;
#4169 = CARTESIAN_POINT ( 'NONE',  ( -24.29636831944148412, 5.264013524081125439, -2.993845543551514776 ) ) ;
#4170 = EDGE_CURVE ( 'NONE', #3172, #477, #6610, .T. ) ;
#4171 = EDGE_CURVE ( 'NONE', #1865, #4629, #6850, .T. ) ;
#4172 = CARTESIAN_POINT ( 'NONE',  ( 6.202282335592980367, -63.50128988325390367, -3.194577187992014622 ) ) ;
#4173 = CARTESIAN_POINT ( 'NONE',  ( 43.95774332523846795, -95.00278575785266355, 2.999999999999905409 ) ) ;
#4174 = VERTEX_POINT ( 'NONE', #7195 ) ;
#4175 = ORIENTED_EDGE ( 'NONE', *, *, #1718, .T. ) ;
#4176 =( NAMED_UNIT ( * ) PLANE_ANGLE_UNIT ( ) SI_UNIT ( $, .RADIAN. ) );
#4177 = CARTESIAN_POINT ( 'NONE',  ( 9.311407240687648468, -51.41373841511900622, -2.502481404895003259 ) ) ;
#4178 = CARTESIAN_POINT ( 'NONE',  ( -17.04733905648494030, -8.234069079964157822, -3.000000000000009326 ) ) ;
#4179 = CARTESIAN_POINT ( 'NONE',  ( 15.04504472124806114, -38.21726078621907874, -3.816391647148975608E-14 ) ) ;
#4180 = LINE ( 'NONE', #1905, #4814 ) ;
#4181 = DIRECTION ( 'NONE',  ( -0.9721221936972339606, -0.2344748185227520099, 0.000000000000000000 ) ) ;
#4182 = ORIENTED_EDGE ( 'NONE', *, *, #6829, .T. ) ;
#4183 = CARTESIAN_POINT ( 'NONE',  ( 4.638831626566389588, -63.05209213275327329, 0.3994218305236152400 ) ) ;
#4184 = DIRECTION ( 'NONE',  ( -0.5224671166576538850, 0.8526594349512809368, 0.000000000000000000 ) ) ;
#4185 = CARTESIAN_POINT ( 'NONE',  ( 4.670395546267172904, -63.95756402795250750, -3.369593122188990542 ) ) ;
#4186 = ORIENTED_EDGE ( 'NONE', *, *, #2776, .F. ) ;
#4187 = DIRECTION ( 'NONE',  ( 0.6513146796332690558, 0.5900073775824551392, -0.4771587602596084055 ) ) ;
#4188 = FACE_OUTER_BOUND ( 'NONE', #3232, .T. ) ;
#4189 = CARTESIAN_POINT ( 'NONE',  ( 35.76131148831677109, 4.835142255982176174, -2.999999999999995559 ) ) ;
#4190 = CARTESIAN_POINT ( 'NONE',  ( 10.77958151816464216, 24.37277465456891079, 3.306154456448493484 ) ) ;
#4191 = CARTESIAN_POINT ( 'NONE',  ( -2.585448123472324777, -55.65377943239024461, 0.04593497335228470535 ) ) ;
#4192 = CYLINDRICAL_SURFACE ( 'NONE', #987, 140.0000000000000284 ) ;
#4193 = CARTESIAN_POINT ( 'NONE',  ( 0.000000000000000000, 0.000000000000000000, 0.000000000000000000 ) ) ;
#4194 = ORIENTED_EDGE ( 'NONE', *, *, #4580, .T. ) ;
#4195 = EDGE_LOOP ( 'NONE', ( #4553, #4490, #3170, #5481 ) ) ;
#4196 = ORIENTED_EDGE ( 'NONE', *, *, #761, .T. ) ;
#4197 = EDGE_CURVE ( 'NONE', #4894, #2728, #3596, .T. ) ;
#4198 = PLANE ( 'NONE',  #2330 ) ;
#4199 = ORIENTED_EDGE ( 'NONE', *, *, #4521, .F. ) ;
#4200 = AXIS2_PLACEMENT_3D ( 'NONE', #1911, #4220, #6513 ) ;
#4201 = DIRECTION ( 'NONE',  ( -0.9721221936972339606, -0.2344748185227520099, 0.000000000000000000 ) ) ;
#4202 = CARTESIAN_POINT ( 'NONE',  ( 5.674632694949170109, -63.26545500802649258, -3.549449971387770297 ) ) ;
#4203 = CYLINDRICAL_SURFACE ( 'NONE', #767, 0.5000000000000004441 ) ;
#4204 = ORIENTED_EDGE ( 'NONE', *, *, #2990, .T. ) ;
#4205 = ORIENTED_EDGE ( 'NONE', *, *, #935, .T. ) ;
#4206 = EDGE_LOOP ( 'NONE', ( #7355, #2837, #1052, #2747 ) ) ;
#4207 = AXIS2_PLACEMENT_3D ( 'NONE', #2257, #3645, #4712 ) ;
#4208 = EDGE_CURVE ( 'NONE', #1675, #3009, #4341, .T. ) ;
#4209 =( LENGTH_UNIT ( ) NAMED_UNIT ( * ) SI_UNIT ( .MILLI., .METRE. ) );
#4210 = LINE ( 'NONE', #5420, #3031 ) ;
#4211 = CARTESIAN_POINT ( 'NONE',  ( -14.97059744062764075, -34.32647288175419931, -2.566271404895000163 ) ) ;
#4212 = VECTOR ( 'NONE', #2135, 1000.000000000000000 ) ;
#4213 = DIRECTION ( 'NONE',  ( -0.9999836672264332815, 0.005715354789842956411, 0.000000000000000000 ) ) ;
#4214 = CARTESIAN_POINT ( 'NONE',  ( -1.974098099753330171, -66.57628266072889289, 3.196874607719439876 ) ) ;
#4215 = ADVANCED_FACE ( 'NONE', ( #5978 ), #5401, .T. ) ;
#4216 = VECTOR ( 'NONE', #6813, 1000.000000000000114 ) ;
#4217 = CARTESIAN_POINT ( 'NONE',  ( 14.18471095241310032, -36.69976849081635351, 2.597518595105000383 ) ) ;
#4218 = CARTESIAN_POINT ( 'NONE',  ( 3.023925381325990092, -64.82443887782423531, -1.545558412227113765 ) ) ;
#4219 = FILL_AREA_STYLE ('',( #2939 ) ) ;
#4220 = DIRECTION ( 'NONE',  ( 5.715354789845005112E-18, 9.999836672264339449E-16, -1.000000000000000000 ) ) ;
#4221 = CARTESIAN_POINT ( 'NONE',  ( 5.790058697650237285, -60.49223513209997094, -1.481755374152989191 ) ) ;
#4222 = ORIENTED_EDGE ( 'NONE', *, *, #2636, .F. ) ;
#4223 = CARTESIAN_POINT ( 'NONE',  ( -9.311346830843410416, -51.41373841511900622, 1.033728595105000148 ) ) ;
#4224 = DIRECTION ( 'NONE',  ( -0.9999836672264333925, 0.005715354789844476896, 0.000000000000000000 ) ) ;
#4225 = FACE_OUTER_BOUND ( 'NONE', #1014, .T. ) ;
#4226 = CARTESIAN_POINT ( 'NONE',  ( 35.41737116972092281, 6.499986109694644298, -1.499999999999993783 ) ) ;
#4227 = CARTESIAN_POINT ( 'NONE',  ( -6.216708800954390490, -58.75440211775612909, 1.606470739968075545 ) ) ;
#4228 = CARTESIAN_POINT ( 'NONE',  ( -24.29636831944148412, 5.264013524081121886, 0.006154456448480109809 ) ) ;
#4229 = ORIENTED_EDGE ( 'NONE', *, *, #4580, .F. ) ;
#4230 = CIRCLE ( 'NONE', #980, 0.7499999999999896749 ) ;
#4231 = VECTOR ( 'NONE', #1491, 1000.000000000000000 ) ;
#4232 = ORIENTED_EDGE ( 'NONE', *, *, #3426, .F. ) ;
#4233 = ORIENTED_EDGE ( 'NONE', *, *, #6248, .F. ) ;
#4234 = LINE ( 'NONE', #3021, #4736 ) ;
#4235 = CIRCLE ( 'NONE', #7357, 0.4999999999999991118 ) ;
#4236 = VECTOR ( 'NONE', #2335, 1000.000000000000000 ) ;
#4237 = LINE ( 'NONE', #4169, #1719 ) ;
#4238 = CARTESIAN_POINT ( 'NONE',  ( 4.666229687490379696, -57.64092629874981810, -1.544454925248829991 ) ) ;
#4239 = AXIS2_PLACEMENT_3D ( 'NONE', #3457, #4562, #494 ) ;
#4240 = EDGE_CURVE ( 'NONE', #5842, #1750, #1435, .T. ) ;
#4241 = ORIENTED_EDGE ( 'NONE', *, *, #1801, .F. ) ;
#4242 = ORIENTED_EDGE ( 'NONE', *, *, #3653, .F. ) ;
#4243 = VECTOR ( 'NONE', #288, 1000.000000000000000 ) ;
#4244 = VERTEX_POINT ( 'NONE', #6674 ) ;
#4245 = EDGE_LOOP ( 'NONE', ( #6897, #4284, #7378, #2359, #1664 ) ) ;
#4246 = VECTOR ( 'NONE', #2761, 1000.000000000000000 ) ;
#4247 = DIRECTION ( 'NONE',  ( -0.8174211450113052502, -0.5760405121937228756, -5.807029557109332903E-16 ) ) ;
#4248 = CIRCLE ( 'NONE', #5224, 2.249999999999996891 ) ;
#4249 = DIRECTION ( 'NONE',  ( 0.000000000000000000, 0.000000000000000000, -1.000000000000000000 ) ) ;
#4250 = VECTOR ( 'NONE', #7240, 1000.000000000000000 ) ;
#4251 = CARTESIAN_POINT ( 'NONE',  ( 5.642462292687943304, -62.26538107922269205, -1.493771565540467305 ) ) ;
#4252 = CARTESIAN_POINT ( 'NONE',  ( 3.219971992657300053, -66.62470095071212484, 2.812725188592500203 ) ) ;
#4253 = EDGE_CURVE ( 'NONE', #7181, #5827, #4330, .T. ) ;
#4254 = B_SPLINE_CURVE_WITH_KNOTS ( 'NONE', 1,
 ( #2028, #5744 ),
 .UNSPECIFIED., .F., .F.,
 ( 2, 2 ),
 ( 0.000000000000000000, 1.000000000000000000 ),
 .UNSPECIFIED. ) ;
#4255 = VECTOR ( 'NONE', #3372, 1000.000000000000000 ) ;
#4256 = PRODUCT_DEFINITION ( 'UNKNOWN', '', #757, #6672 ) ;
#4257 = DIRECTION ( 'NONE',  ( 0.9999836672264331705, -0.005715354789860001804, 0.000000000000000000 ) ) ;
#4258 = CARTESIAN_POINT ( 'NONE',  ( -1.241878142352246028, -55.26848170174031338, 1.724521099399885182 ) ) ;
#4259 = AXIS2_PLACEMENT_3D ( 'NONE', #2943, #6417, #1262 ) ;
#4260 =( GEOMETRIC_REPRESENTATION_CONTEXT ( 3 ) GLOBAL_UNCERTAINTY_ASSIGNED_CONTEXT ( ( #797 ) ) GLOBAL_UNIT_ASSIGNED_CONTEXT ( ( #6381, #3076, #6349 ) ) REPRESENTATION_CONTEXT ( 'NONE', 'WORKASPACE' ) );
#4261 = CARTESIAN_POINT ( 'NONE',  ( 14.49911764349215915, -35.75048010860329839, 0.4975185951050001831 ) ) ;
#4262 = FACE_OUTER_BOUND ( 'NONE', #5768, .T. ) ;
#4263 = EDGE_CURVE ( 'NONE', #7025, #878, #2751, .T. ) ;
#4264 = EDGE_CURVE ( 'NONE', #4598, #3100, #1557, .T. ) ;
#4265 = CARTESIAN_POINT ( 'NONE',  ( 0.06232375252353471867, -54.65437704685372466, -2.006095305823016428 ) ) ;
#4266 = AXIS2_PLACEMENT_3D ( 'NONE', #3801, #1654, #5169 ) ;
#4267 = ORIENTED_EDGE ( 'NONE', *, *, #7135, .F. ) ;
#4268 = CARTESIAN_POINT ( 'NONE',  ( 104.0973215944787711, -119.5240462704291389, -3.000000000000119904 ) ) ;
#4269 = DIRECTION ( 'NONE',  ( 0.1860016876085203441, -0.1636620475539279917, 0.9688230521603200529 ) ) ;
#4270 = DIRECTION ( 'NONE',  ( 5.715354789845005112E-18, 9.999836672264339449E-16, -1.000000000000000000 ) ) ;
#4271 = DIRECTION ( 'NONE',  ( 0.000000000000000000, 0.000000000000000000, -1.000000000000000000 ) ) ;
#4272 = EDGE_CURVE ( 'NONE', #4165, #6113, #5782, .T. ) ;
#4273 = CARTESIAN_POINT ( 'NONE',  ( 1.700848490796859958, -66.65813550864595527, 0.8993149516912349872 ) ) ;
#4274 = CARTESIAN_POINT ( 'NONE',  ( 5.854317997614909785, -64.22630450538810010, 2.635376777014039718 ) ) ;
#4275 = DIRECTION ( 'NONE',  ( 0.000000000000000000, 0.000000000000000000, -1.000000000000000000 ) ) ;
#4276 = ORIENTED_EDGE ( 'NONE', *, *, #7286, .T. ) ;
#4277 = ORIENTED_EDGE ( 'NONE', *, *, #1928, .F. ) ;
#4278 = VERTEX_POINT ( 'NONE', #2783 ) ;
#4279 = CARTESIAN_POINT ( 'NONE',  ( -7.741417275248890562, 12.33509147838778475, 3.000000000000011990 ) ) ;
#4280 = DIRECTION ( 'NONE',  ( -0.4039838799357114985, -0.9147661038495515928, -8.673617379884191272E-16 ) ) ;
#4281 = CARTESIAN_POINT ( 'NONE',  ( -4.739687333205909958, -61.73825078254577647, 2.268939929871689909 ) ) ;
#4282 = CARTESIAN_POINT ( 'NONE',  ( -5.737183749403212296, -62.91840231736271960, 3.479437450128457954 ) ) ;
#4283 = VERTEX_POINT ( 'NONE', #5102 ) ;
#4284 = ORIENTED_EDGE ( 'NONE', *, *, #3975, .T. ) ;
#4285 = ORIENTED_EDGE ( 'NONE', *, *, #6428, .T. ) ;
#4286 = DIRECTION ( 'NONE',  ( 1.000000000000000000, 0.000000000000000000, 0.000000000000000000 ) ) ;
#4287 = CARTESIAN_POINT ( 'NONE',  ( 43.95483829995806957, -94.87490738911687060, -3.001370543551634906 ) ) ;
#4288 = PRODUCT_DEFINITION_SHAPE ( 'NONE', 'NONE',  #4256 ) ;
#4289 = CARTESIAN_POINT ( 'NONE',  ( 41.70778007397900211, -94.98992620957551480, 2.999999999999905409 ) ) ;
#4290 = CARTESIAN_POINT ( 'NONE',  ( -12.10129460565897475, -12.45149060151658382, -1.252045042622798671E-14 ) ) ;
#4291 = CARTESIAN_POINT ( 'NONE',  ( 1.830733139179690161, -67.16965779809959258, 0.7798461408577649356 ) ) ;
#4292 = EDGE_LOOP ( 'NONE', ( #3886, #415, #6647, #4491 ) ) ;
#4293 = ORIENTED_EDGE ( 'NONE', *, *, #3556, .T. ) ;
#4294 = EDGE_CURVE ( 'NONE', #4944, #4040, #3233, .T. ) ;
#4295 = CARTESIAN_POINT ( 'NONE',  ( 19.86817077757007510, -41.71399671145084653, -4.163336342344337027E-14 ) ) ;
#4296 = CARTESIAN_POINT ( 'NONE',  ( 5.677676720488819662, -58.78440004686129328, 0.4885712913175552785 ) ) ;
#4297 = FACE_OUTER_BOUND ( 'NONE', #5877, .T. ) ;
#4298 = CARTESIAN_POINT ( 'NONE',  ( -13.19674249314596892, -2.997380612392111843, -3.000000000000003997 ) ) ;
#4299 = CARTESIAN_POINT ( 'NONE',  ( -2.621169780003727467, -55.22978393027467803, -0.06561799439619847574 ) ) ;
#4300 = VERTEX_POINT ( 'NONE', #3202 ) ;
#4301 = DIRECTION ( 'NONE',  ( 0.8688689365825388311, 0.4950421911735690128, 0.000000000000000000 ) ) ;
#4302 = EDGE_CURVE ( 'NONE', #5560, #3333, #5178, .T. ) ;
#4303 = EDGE_CURVE ( 'NONE', #4319, #3409, #2679, .T. ) ;
#4304 = FACE_OUTER_BOUND ( 'NONE', #6191, .T. ) ;
#4305 = CARTESIAN_POINT ( 'NONE',  ( -14.38395162568175145, 6.352317343304507702, 6.270004205522762891E-15 ) ) ;
#4306 = CARTESIAN_POINT ( 'NONE',  ( 6.162074140922939591, -62.32076522084695114, 2.666565443060120444 ) ) ;
#4307 = CARTESIAN_POINT ( 'NONE',  ( -6.841972559203830961, -62.34857902771452842, 2.832214187714990228 ) ) ;
#4308 = FACE_OUTER_BOUND ( 'NONE', #6607, .T. ) ;
#4309 = EDGE_LOOP ( 'NONE', ( #3192, #2842, #2201, #2732, #2277, #3546 ) ) ;
#4310 = VERTEX_POINT ( 'NONE', #2228 ) ;
#4311 = EDGE_LOOP ( 'NONE', ( #6282, #6697, #1676, #3960 ) ) ;
#4312 = ADVANCED_FACE ( 'NONE', ( #1627 ), #1065, .F. ) ;
#4313 = CARTESIAN_POINT ( 'NONE',  ( 27.65533861039811114, -36.12687000486603495, 2.999999999999964029 ) ) ;
#4314 = CARTESIAN_POINT ( 'NONE',  ( 12.40979888490706706, -30.61452125107580713, -3.035766082959412415E-14 ) ) ;
#4315 = CARTESIAN_POINT ( 'NONE',  ( -4.892892059336399591, -61.27075929137718191, 2.302341147961269652 ) ) ;
#4316 = DIRECTION ( 'NONE',  ( 0.3128416502900965290, -0.9445788350777319931, 0.09950339776592478924 ) ) ;
#4317 = CARTESIAN_POINT ( 'NONE',  ( 5.012342441489318290, -56.71631922511256363, 2.351956307816288394 ) ) ;
#4318 = ORIENTED_EDGE ( 'NONE', *, *, #1132, .T. ) ;
#4319 = VERTEX_POINT ( 'NONE', #4986 ) ;
#4320 = APPLICATION_PROTOCOL_DEFINITION ( 'draft international standard', 'automotive_design', 1998, #6403 ) ;
#4321 = CARTESIAN_POINT ( 'NONE',  ( -19.59526946576633222, 14.55287597139389888, 0.006154456448479242447 ) ) ;
#4322 = CARTESIAN_POINT ( 'NONE',  ( 14.07443455944474131, -37.03272609524245240, -0.9950371902099899302 ) ) ;
#4323 = CARTESIAN_POINT ( 'NONE',  ( 11.49981217310398485, -0.06572658008321753675, 3.000000000000000000 ) ) ;
#4324 = CARTESIAN_POINT ( 'NONE',  ( 1.402950248545461909, -54.15620739517822813, 0.01614447287717020105 ) ) ;
#4325 = ORIENTED_EDGE ( 'NONE', *, *, #5421, .F. ) ;
#4326 = VECTOR ( 'NONE', #5014, 1000.000000000000000 ) ;
#4327 = EDGE_LOOP ( 'NONE', ( #587, #1562, #2588, #5129 ) ) ;
#4328 = DIRECTION ( 'NONE',  ( 0.9147661038495522590, -0.4039838799357101107, 0.000000000000000000 ) ) ;
#4329 = CARTESIAN_POINT ( 'NONE',  ( -2.607408651135029842, -55.80429912246091106, 1.635486251833709881 ) ) ;
#4330 = CIRCLE ( 'NONE', #6026, 1.000000000000001776 ) ;
#4331 = ORIENTED_EDGE ( 'NONE', *, *, #3556, .F. ) ;
#4332 = CARTESIAN_POINT ( 'NONE',  ( 15.94457129749017277, -41.07922723232461237, -4.119968255444916849E-14 ) ) ;
#4333 = DIRECTION ( 'NONE',  ( -0.8856191127862077517, -0.4644123028815776988, -4.694663451788343547E-16 ) ) ;
#4334 = EDGE_CURVE ( 'NONE', #3385, #1522, #464, .T. ) ;
#4335 = AXIS2_PLACEMENT_3D ( 'NONE', #2827, #5709, #1747 ) ;
#4336 = ORIENTED_EDGE ( 'NONE', *, *, #1363, .T. ) ;
#4337 = DIRECTION ( 'NONE',  ( 5.715354789845005112E-18, 9.999836672264339449E-16, -1.000000000000000000 ) ) ;
#4338 = CIRCLE ( 'NONE', #3491, 1.000000000000000888 ) ;
#4339 = CARTESIAN_POINT ( 'NONE',  ( 22.09517004029793696, 21.09482167756528526, -1.493845543551514332 ) ) ;
#4340 = CARTESIAN_POINT ( 'NONE',  ( 11.49981217310398485, -0.06572658008321453915, 0.000000000000000000 ) ) ;
#4341 = LINE ( 'NONE', #6629, #4451 ) ;
#4342 = DIRECTION ( 'NONE',  ( 0.6713653717953965705, -0.7411265327553918647, -7.095217611944926095E-16 ) ) ;
#4343 = CARTESIAN_POINT ( 'NONE',  ( 5.919885402076849878, -56.76393675504415626, 0.1623732496884200682 ) ) ;
#4344 = ADVANCED_FACE ( 'NONE', ( #947 ), #3238, .F. ) ;
#4345 = DIRECTION ( 'NONE',  ( 0.9999836672264332815, -0.005715354789860001804, 0.000000000000000000 ) ) ;
#4346 = EDGE_CURVE ( 'NONE', #5242, #3657, #5665, .T. ) ;
#4347 = ORIENTED_EDGE ( 'NONE', *, *, #3336, .F. ) ;
#4348 = EDGE_LOOP ( 'NONE', ( #3935, #3429 ) ) ;
#4349 = DIRECTION ( 'NONE',  ( 5.715354789860003484E-18, 9.999836672264337477E-16, -1.000000000000000000 ) ) ;
#4350 = CARTESIAN_POINT ( 'NONE',  ( 8.553800617183139110, 16.61347289177635034, -0.1384873327366685780 ) ) ;
#4351 = CARTESIAN_POINT ( 'NONE',  ( 0.9735761768007340500, -65.42433328568066031, 1.767115439505955177 ) ) ;
#4352 = CARTESIAN_POINT ( 'NONE',  ( 18.47982041150265431, -39.47532202006953383, 2.999999999999960476 ) ) ;
#4353 = EDGE_CURVE ( 'NONE', #2276, #888, #5556, .T. ) ;
#4354 = CARTESIAN_POINT ( 'NONE',  ( -3.638963596321122651, -65.59027719068511431, 3.295737659246797957 ) ) ;
#4355 = EDGE_CURVE ( 'NONE', #6505, #7060, #2715, .T. ) ;
#4356 = CARTESIAN_POINT ( 'NONE',  ( 4.520351875826989385, -63.47384446676466752, 0.9302720625520102260 ) ) ;
#4357 = EDGE_LOOP ( 'NONE', ( #4769, #268, #667 ) ) ;
#4358 = ORIENTED_EDGE ( 'NONE', *, *, #7011, .F. ) ;
#4359 = VERTEX_POINT ( 'NONE', #4947 ) ;
#4360 = CIRCLE ( 'NONE', #4735, 1.100000000000000755 ) ;
#4361 = CIRCLE ( 'NONE', #2666, 0.9999999999999998890 ) ;
#4362 =( NAMED_UNIT ( * ) SI_UNIT ( $, .STERADIAN. ) SOLID_ANGLE_UNIT ( ) );
#4363 = CARTESIAN_POINT ( 'NONE',  ( -12.20412794045469518, -35.68083184586667045, -3.000000000000036415 ) ) ;
#4364 = DIRECTION ( 'NONE',  ( -0.9721221936972339606, -0.2344748185227520099, 0.000000000000000000 ) ) ;
#4365 = LINE ( 'NONE', #897, #6651 ) ;
#4366 = CARTESIAN_POINT ( 'NONE',  ( 5.919885402076849878, -56.76393675504415626, 0.1623732496884200682 ) ) ;
#4367 = VECTOR ( 'NONE', #4090, 1000.000000000000114 ) ;
#4368 = VECTOR ( 'NONE', #3458, 999.9999999999998863 ) ;
#4369 = VECTOR ( 'NONE', #2333, 1000.000000000000114 ) ;
#4370 = ORIENTED_EDGE ( 'NONE', *, *, #6468, .T. ) ;
#4371 = DIRECTION ( 'NONE',  ( 0.2223191033124284066, 0.6712482523644728305, 0.7071067811865466846 ) ) ;
#4372 = AXIS2_PLACEMENT_3D ( 'NONE', #4773, #3629, #3700 ) ;
#4373 = CARTESIAN_POINT ( 'NONE',  ( -5.354034084503060065, -64.02545556441495478, -0.7792797212839647214 ) ) ;
#4374 = AXIS2_PLACEMENT_3D ( 'NONE', #5004, #4435, #2123 ) ;
#4375 = AXIS2_PLACEMENT_3D ( 'NONE', #2439, #2916, #4677 ) ;
#4376 = CARTESIAN_POINT ( 'NONE',  ( -10.26063678088237907, -51.72814037242050489, 2.533728595105000370 ) ) ;
#4377 = DIRECTION ( 'NONE',  ( -5.715354789845005112E-18, -9.999836672264339449E-16, 1.000000000000000000 ) ) ;
#4378 = VERTEX_POINT ( 'NONE', #3839 ) ;
#4379 = CIRCLE ( 'NONE', #5472, 0.5000000000000004441 ) ;
#4380 = AXIS2_PLACEMENT_3D ( 'NONE', #3203, #2108, #4915 ) ;
#4381 = PRODUCT_RELATED_PRODUCT_CATEGORY ( 'part', '', ( #729 ) ) ;
#4382 = CARTESIAN_POINT ( 'NONE',  ( 0.000000000000000000, 0.000000000000000000, -17.67054229618195293 ) ) ;
#4383 = CARTESIAN_POINT ( 'NONE',  ( -33.25476684253234794, 13.81160679460617757, -1.499999999999986899 ) ) ;
#4384 = CARTESIAN_POINT ( 'NONE',  ( 1.714606436953501688E-17, 2.999951001679301835E-15, 0.000000000000000000 ) ) ;
#4385 = DIRECTION ( 'NONE',  ( -0.08966155106958693943, -0.9959722919136836383, 0.000000000000000000 ) ) ;
#4386 = AXIS2_PLACEMENT_3D ( 'NONE', #1096, #497, #6670 ) ;
#4387 = DIRECTION ( 'NONE',  ( -0.9999836672264335036, 0.005715354789845008589, 0.000000000000000000 ) ) ;
#4388 = CARTESIAN_POINT ( 'NONE',  ( -6.177752788274950113, -57.21669580536380550, -0.5454192084659099660 ) ) ;
#4389 = LINE ( 'NONE', #1106, #6042 ) ;
#4390 = ORIENTED_EDGE ( 'NONE', *, *, #4909, .T. ) ;
#4391 = EDGE_LOOP ( 'NONE', ( #6991, #2199, #2621, #6796 ) ) ;
#4392 = ADVANCED_FACE ( 'NONE', ( #6158 ), #7332, .T. ) ;
#4393 = FACE_OUTER_BOUND ( 'NONE', #2470, .T. ) ;
#4394 = PLANE ( 'NONE',  #397 ) ;
#4395 = CARTESIAN_POINT ( 'NONE',  ( -2.954381708604445045, -64.87272166844897470, 3.050067095118260241 ) ) ;
#4396 = CARTESIAN_POINT ( 'NONE',  ( 27.30483170388657044, -34.44723004512044895, 2.999999999999965805 ) ) ;
#4397 = CARTESIAN_POINT ( 'NONE',  ( 6.229763166278965869, -60.90327177492465438, 0.4901581683790414701 ) ) ;
#4398 = ORIENTED_EDGE ( 'NONE', *, *, #1031, .T. ) ;
#4399 = ORIENTED_EDGE ( 'NONE', *, *, #1437, .F. ) ;
#4400 = ORIENTED_EDGE ( 'NONE', *, *, #7152, .F. ) ;
#4401 = ORIENTED_EDGE ( 'NONE', *, *, #7328, .T. ) ;
#4402 = EDGE_CURVE ( 'NONE', #4757, #2710, #5020, .T. ) ;
#4403 = EDGE_CURVE ( 'NONE', #3934, #6387, #6613, .T. ) ;
#4404 = DIRECTION ( 'NONE',  ( 0.3144019573014847913, -0.9492899500389727629, 0.000000000000000000 ) ) ;
#4405 = DIRECTION ( 'NONE',  ( -5.715354789860003484E-18, -9.999836672264337477E-16, 1.000000000000000000 ) ) ;
#4406 = DIRECTION ( 'NONE',  ( -5.715354789845133764E-18, -9.999836672264337477E-16, 1.000000000000000000 ) ) ;
#4407 = CARTESIAN_POINT ( 'NONE',  ( 1.414957918137925930, -67.26958221326191278, 2.900267041832249593 ) ) ;
#4408 = EDGE_LOOP ( 'NONE', ( #3762, #4062, #1303, #3898 ) ) ;
#4409 = DIRECTION ( 'NONE',  ( -0.9793199139485103677, -0.2023178344681514362, -2.079116908177635377E-16 ) ) ;
#4410 = ADVANCED_BREP_SHAPE_REPRESENTATION ( '', ( #4713, #751 ), #2789 ) ;
#4411 = CARTESIAN_POINT ( 'NONE',  ( 5.416018991692120643, -63.93240027730202968, 2.754852738177090643 ) ) ;
#4412 = DIRECTION ( 'NONE',  ( 5.715354789845005112E-18, 9.999836672264339449E-16, -1.000000000000000000 ) ) ;
#4413 = DIRECTION ( 'NONE',  ( -5.715354789845005112E-18, -9.999836672264339449E-16, 1.000000000000000000 ) ) ;
#4414 = B_SPLINE_CURVE_WITH_KNOTS ( 'NONE', 3,
 ( #808, #4282, #2008, #5533, #4926, #4354, #6134, #6606, #6102, #2540, #6645, #2617, #3813, #1492, #3702, #2403, #4714, #2090, #839, #4847, #4317, #5885, #3780, #6997, #3097, #1842, #5503, #3213, #3738, #1447, #3177, #4959, #926, #3250, #361, #3570, #3134, #887, #1290, #326, #7208, #6021, #4147, #7246, #6444, #5453, #2044, #1970, #290, #2652, #7136, #4397, #6685, #959, #1527, #2584, #5413, #247, #113, #4890, #6573, #1413, #7171, #6063, #402, #999, #7279, #3365, #1116, #1639, #7353, #1076, #2836, #1673, #1160, #4547, #1561, #1041, #6242, #6717, #5677, #2273, #1607, #2118, #5153 ),
 .UNSPECIFIED., .F., .F.,
 ( 4, 2, 2, 1, 2, 2, 2, 2, 2, 2, 1, 2, 2, 2, 2, 2, 2, 1, 2, 2, 2, 2, 1, 2, 2, 2, 2, 2, 2, 1, 2, 2, 2, 2, 2, 2, 1, 2, 2, 2, 2, 2, 2, 1, 2, 4 ),
 ( 0.000000000000000000, 0.01562500000000017347, 0.03125000000000034694, 0.06250000000000038858, 0.07812500000000047184, 0.09375000000000056899, 0.1250000000000006661, 0.1406250000000005829, 0.1562500000000004996, 0.1875000000000007772, 0.2187500000000010270, 0.2343750000000011657, 0.2500000000000012768, 0.2812500000000013878, 0.2968750000000014433, 0.3125000000000014988, 0.3437500000000017208, 0.3750000000000018874, 0.3906250000000019429, 0.4062500000000019984, 0.4375000000000021649, 0.4531250000000021094, 0.4687500000000019984, 0.5000000000000017764, 0.5312500000000016653, 0.5468750000000017764, 0.5625000000000017764, 0.5937500000000017764, 0.6093750000000017764, 0.6250000000000016653, 0.6562500000000015543, 0.6875000000000013323, 0.7031250000000012212, 0.7187500000000012212, 0.7500000000000009992, 0.7656250000000009992, 0.7812500000000008882, 0.8125000000000007772, 0.8437500000000006661, 0.8593750000000005551, 0.8750000000000003331, 0.9062500000000003331, 0.9218750000000002220, 0.9375000000000002220, 0.9687500000000001110, 1.000000000000000000 ),
 .UNSPECIFIED. ) ;
#4415 = EDGE_LOOP ( 'NONE', ( #1927, #1679, #5568, #6465 ) ) ;
#4416 = EDGE_CURVE ( 'NONE', #7272, #3172, #2895, .T. ) ;
#4417 = CYLINDRICAL_SURFACE ( 'NONE', #2779, 1.100000000000000755 ) ;
#4418 = LINE ( 'NONE', #1548, #4743 ) ;
#4419 = DIRECTION ( 'NONE',  ( 0.8481698128690331462, -0.5297244269785085224, -5.248681837068071230E-16 ) ) ;
#4420 = DIRECTION ( 'NONE',  ( 0.8688689365825387201, 0.4950421911735688463, 4.999999999999993486E-16 ) ) ;
#4421 = CARTESIAN_POINT ( 'NONE',  ( -6.362523631248359735, -64.09785492953841413, 0.6509934082767404595 ) ) ;
#4422 = FACE_OUTER_BOUND ( 'NONE', #1310, .T. ) ;
#4423 = ORIENTED_EDGE ( 'NONE', *, *, #1437, .T. ) ;
#4424 = CARTESIAN_POINT ( 'NONE',  ( 14.63763862841553376, 20.11382921380833011, -2.993845543551509447 ) ) ;
#4425 = CARTESIAN_POINT ( 'NONE',  ( -16.40387102536037744, 1.778486824056639826, 1.734723475976807094E-15 ) ) ;
#4426 = CARTESIAN_POINT ( 'NONE',  ( 9.311407240687648468, -51.41373841511902043, -1.002481404894999928 ) ) ;
#4427 = CARTESIAN_POINT ( 'NONE',  ( 1.576955190785845007, -65.26733347271304808, -2.474060432887700500 ) ) ;
#4428 = CARTESIAN_POINT ( 'NONE',  ( -22.27644891976294161, 9.837844043328900057, 3.306154456448478829 ) ) ;
#4429 = DIRECTION ( 'NONE',  ( -0.4950421911735701785, 0.8688689365825380539, 8.521476159766246785E-16 ) ) ;
#4430 = ORIENTED_EDGE ( 'NONE', *, *, #15, .F. ) ;
#4431 = ADVANCED_FACE ( 'NONE', ( #5216 ), #88, .F. ) ;
#4432 = ORIENTED_EDGE ( 'NONE', *, *, #2905, .F. ) ;
#4433 = ORIENTED_EDGE ( 'NONE', *, *, #4653, .F. ) ;
#4434 = DIRECTION ( 'NONE',  ( 0.000000000000000000, 0.000000000000000000, 1.000000000000000000 ) ) ;
#4435 = DIRECTION ( 'NONE',  ( -0.9147661038495488173, 0.4039838799357178822, 0.000000000000000000 ) ) ;
#4436 = CARTESIAN_POINT ( 'NONE',  ( -14.49899450467539985, -35.75040780681265318, -2.566271404894997499 ) ) ;
#4437 = DIRECTION ( 'NONE',  ( -5.715354789860003484E-18, -9.999836672264337477E-16, 1.000000000000000000 ) ) ;
#4438 = CARTESIAN_POINT ( 'NONE',  ( -6.994430249510970476, -62.66069223349322925, -1.382237850844937777 ) ) ;
#4439 = EDGE_LOOP ( 'NONE', ( #3304, #2525, #4087 ) ) ;
#4440 = EDGE_CURVE ( 'NONE', #5957, #5943, #4704, .T. ) ;
#4441 = EDGE_CURVE ( 'NONE', #5643, #5379, #4656, .T. ) ;
#4442 = ORIENTED_EDGE ( 'NONE', *, *, #1963, .T. ) ;
#4443 = DIRECTION ( 'NONE',  ( -0.4039838799357176602, -0.9147661038495489283, -9.170600743851254660E-16 ) ) ;
#4444 = DIRECTION ( 'NONE',  ( -5.715354789845005112E-18, -9.999836672264339449E-16, 1.000000000000000000 ) ) ;
#4445 = CARTESIAN_POINT ( 'NONE',  ( -3.235261603508409856, -66.01500717273368934, 1.164464255201294929 ) ) ;
#4446 = AXIS2_PLACEMENT_3D ( 'NONE', #2711, #7298, #3424 ) ;
#4447 = DIRECTION ( 'NONE',  ( 0.9858503002877112564, -0.1676281164441980331, -1.619908943762944784E-16 ) ) ;
#4448 = DIRECTION ( 'NONE',  ( 0.9999836672264332815, -0.005715354789859183882, 0.000000000000000000 ) ) ;
#4449 = EDGE_CURVE ( 'NONE', #6990, #6323, #3999, .T. ) ;
#4450 = EDGE_LOOP ( 'NONE', ( #928, #6004 ) ) ;
#4451 = VECTOR ( 'NONE', #3662, 1000.000000000000227 ) ;
#4452 = CARTESIAN_POINT ( 'NONE',  ( 18.05682814888138665, -39.71632386479095089, 3.883467497571597704 ) ) ;
#4453 = CARTESIAN_POINT ( 'NONE',  ( -12.75609440306747189, -34.09959597428994726, -3.000000000000035083 ) ) ;
#4454 = DIRECTION ( 'NONE',  ( 0.9999836672264332815, -0.005715354789845002517, 0.000000000000000000 ) ) ;
#4455 = VECTOR ( 'NONE', #4333, 1000.000000000000114 ) ;
#4456 = CARTESIAN_POINT ( 'NONE',  ( 3.455862201155819768, -54.25194821296495462, -1.605226101400722083 ) ) ;
#4457 = CARTESIAN_POINT ( 'NONE',  ( -19.77196556206555655, 3.265922675912619866, 2.236547809770379480 ) ) ;
#4458 = ORIENTED_EDGE ( 'NONE', *, *, #3098, .T. ) ;
#4459 = DIRECTION ( 'NONE',  ( -5.715354789845005112E-18, -9.999836672264339449E-16, 1.000000000000000000 ) ) ;
#4460 = SHAPE_REPRESENTATION ( 'Pliers Right Handle Arm', ( #751 ), #2789 ) ;
#4461 = CARTESIAN_POINT ( 'NONE',  ( 0.9735761768007340500, -65.42433328568066031, 1.767115439505955177 ) ) ;
#4462 = CARTESIAN_POINT ( 'NONE',  ( 10.46182022341160867, 4.774967812772744402, 4.770489558936219510E-15 ) ) ;
#4463 = CARTESIAN_POINT ( 'NONE',  ( 12.99837876291259064, -32.41640519645540053, 2.999999999999967581 ) ) ;
#4464 = CARTESIAN_POINT ( 'NONE',  ( -5.155987128177820900, -61.76400128369626685, 1.194474120832875519 ) ) ;
#4465 = LINE ( 'NONE', #2239, #2066 ) ;
#4466 = DIRECTION ( 'NONE',  ( -0.9147661038495521479, 0.4039838799357104993, 3.987490689252507167E-16 ) ) ;
#4467 = ORIENTED_EDGE ( 'NONE', *, *, #5784, .T. ) ;
#4468 = ORIENTED_EDGE ( 'NONE', *, *, #943, .T. ) ;
#4469 = ORIENTED_EDGE ( 'NONE', *, *, #2305, .T. ) ;
#4470 = DIRECTION ( 'NONE',  ( 0.9999836672264333925, -0.005715354789844381486, 0.000000000000000000 ) ) ;
#4471 = ORIENTED_EDGE ( 'NONE', *, *, #5502, .F. ) ;
#4472 = CLOSED_SHELL ( 'NONE', ( #2806, #209, #302 ) ) ;
#4473 = EDGE_CURVE ( 'NONE', #4852, #4770, #5059, .T. ) ;
#4474 = FILL_AREA_STYLE ('',( #483 ) ) ;
#4475 = PLANE ( 'NONE',  #5462 ) ;
#4476 = CARTESIAN_POINT ( 'NONE',  ( 26.13478801451176636, 24.75419629621026019, -1.493845543551509891 ) ) ;
#4477 = CARTESIAN_POINT ( 'NONE',  ( -6.362523631248359735, -64.09785492953841413, 0.6509934082767404595 ) ) ;
#4478 = VERTEX_POINT ( 'NONE', #6414 ) ;
#4479 = ORIENTED_EDGE ( 'NONE', *, *, #7190, .T. ) ;
#4480 = CIRCLE ( 'NONE', #3529, 3.750000000000000444 ) ;
#4481 = AXIS2_PLACEMENT_3D ( 'NONE', #5606, #6062, #4181 ) ;
#4482 = CARTESIAN_POINT ( 'NONE',  ( -95.86211798318534250, -102.0316339954322018, -1.025655255171287195E-13 ) ) ;
#4483 = PLANE ( 'NONE',  #44 ) ;
#4484 = CARTESIAN_POINT ( 'NONE',  ( -5.628700163094269016, -63.23550210468251009, 3.461537593744290042 ) ) ;
#4485 = ADVANCED_FACE ( 'NONE', ( #2379 ), #5255, .T. ) ;
#4486 = AXIS2_PLACEMENT_3D ( 'NONE', #3163, #5488, #7192 ) ;
#4487 = CIRCLE ( 'NONE', #1595, 1.100000000000000755 ) ;
#4488 = CARTESIAN_POINT ( 'NONE',  ( -1.172374092613760688, 4.860610968486169803, -3.500000000000000000 ) ) ;
#4489 = DIRECTION ( 'NONE',  ( -0.6713653717953972366, 0.7411265327553915316, 8.596159621131687339E-16 ) ) ;
#4490 = ORIENTED_EDGE ( 'NONE', *, *, #7227, .F. ) ;
#4491 = ORIENTED_EDGE ( 'NONE', *, *, #1269, .F. ) ;
#4492 = AXIS2_PLACEMENT_3D ( 'NONE', #5530, #4923, #2041 ) ;
#4493 = CIRCLE ( 'NONE', #2914, 140.0000000000000284 ) ;
#4494 = AXIS2_PLACEMENT_3D ( 'NONE', #3297, #6108, #3254 ) ;
#4495 = EDGE_CURVE ( 'NONE', #3331, #4841, #1261, .T. ) ;
#4496 = CARTESIAN_POINT ( 'NONE',  ( 18.11932642638120328, -39.68071517522289327, 3.251954915088070663 ) ) ;
#4497 = EDGE_CURVE ( 'NONE', #2788, #6066, #6855, .T. ) ;
#4498 = CARTESIAN_POINT ( 'NONE',  ( 12.15447797363371052, 11.01039466689934088, 3.000000000000011546 ) ) ;
#4499 = AXIS2_PLACEMENT_3D ( 'NONE', #3362, #1668, #4009 ) ;
#4500 = CARTESIAN_POINT ( 'NONE',  ( 14.49911764349215915, -35.75048010860329839, 2.597518595105000383 ) ) ;
#4501 = CIRCLE ( 'NONE', #1931, 0.7500000000000000000 ) ;
#4502 = CARTESIAN_POINT ( 'NONE',  ( 1.894024985814124928, -67.53311321014548696, 0.2080693458549401353 ) ) ;
#4503 = CARTESIAN_POINT ( 'NONE',  ( 9.358334193258830425, -51.27205182843857045, -2.495037190209989930 ) ) ;
#4504 = AXIS2_PLACEMENT_3D ( 'NONE', #5781, #4614, #155 ) ;
#4505 = AXIS2_PLACEMENT_3D ( 'NONE', #1772, #3460, #4145 ) ;
#4506 = EDGE_LOOP ( 'NONE', ( #1428, #5621, #3067, #6262 ) ) ;
#4507 = CARTESIAN_POINT ( 'NONE',  ( -35.54168210215660650, 14.82156649444490348, -0.7500000000019999558 ) ) ;
#4508 = CARTESIAN_POINT ( 'NONE',  ( -4.461725341067024786, -62.58642870417541104, 2.208339520507450082 ) ) ;
#4509 = CARTESIAN_POINT ( 'NONE',  ( 14.49911764349215915, -35.75048010860329839, 2.597518595105000383 ) ) ;
#4510 = CARTESIAN_POINT ( 'NONE',  ( 18.47982041150265786, -39.47532202006954094, -0.5000000000000394129 ) ) ;
#4511 = CARTESIAN_POINT ( 'NONE',  ( 2.735691016399460107, -56.17047939608508500, 0.9718516700694501687 ) ) ;
#4512 = CARTESIAN_POINT ( 'NONE',  ( 26.98474422010017904, -34.62960140479226112, 4.001293834245286618 ) ) ;
#4513 = CARTESIAN_POINT ( 'NONE',  ( 24.99346688245966419, 26.01411140189437532, -2.993845543551503674 ) ) ;
#4514 =( BOUNDED_SURFACE ( )  B_SPLINE_SURFACE ( 3, 2, ( 
 ( #344, #7417, #502 ),
 ( #1181, #6307, #4568 ),
 ( #1625, #7302, #3464 ),
 ( #6902, #4452, #1063 ),
 ( #462, #5098, #4041 ),
 ( #6856, #1027, #1700 ),
 ( #4496, #3996, #3430 ),
 ( #6341, #5056, #2742 ),
 ( #5707, #5742, #5172 ),
 ( #2226, #3876, #3917 ) ),
 .UNSPECIFIED., .F., .F., .F. ) 
 B_SPLINE_SURFACE_WITH_KNOTS ( ( 4, 2, 2, 2, 4 ),
 ( 3, 3 ),
 ( 0.000000000000000000, 0.0001953596913251163321, 0.0003907193826502326642, 0.0005860790739753490505, 0.0007814387653004653284 ),
 ( 0.000000000000000000, 1.000000000000000000 ),
 .UNSPECIFIED. ) 
 GEOMETRIC_REPRESENTATION_ITEM ( )  RATIONAL_B_SPLINE_SURFACE ( (
 ( 1.000000000000000000, 0.7071067811865465735, 1.000000000000000000),
 ( 1.000000000000000000, 0.7051297887126681818, 1.000000000000000000),
 ( 1.000000000000000000, 0.7031405235181358293, 1.000000000000000000),
 ( 1.000000000000000000, 0.6994400710090995510, 1.000000000000000000),
 ( 1.000000000000000000, 0.6977350462886972027, 1.000000000000000000),
 ( 1.000000000000000000, 0.6948874123953024950, 1.000000000000000000),
 ( 1.000000000000000000, 0.6937311395898003719, 1.000000000000000000),
 ( 1.000000000000000000, 0.6921794382103451104, 1.000000000000000000),
 ( 1.000000000000000000, 0.6917621249165484265, 1.000000000000000000),
 ( 1.000000000000000000, 0.6917656125192588323, 1.000000000000000000) ) ) 
 REPRESENTATION_ITEM ( '' )  SURFACE ( )  );
#4515 = CARTESIAN_POINT ( 'NONE',  ( -4.450126406946254498, -63.33667035482537244, 1.592103300391294773 ) ) ;
#4516 = ORIENTED_EDGE ( 'NONE', *, *, #4570, .T. ) ;
#4517 = VECTOR ( 'NONE', #2013, 1000.000000000000000 ) ;
#4518 = EDGE_LOOP ( 'NONE', ( #2002, #3914 ) ) ;
#4519 = ORIENTED_EDGE ( 'NONE', *, *, #1132, .F. ) ;
#4520 = CARTESIAN_POINT ( 'NONE',  ( -44.78727511552453677, -94.39397278840091587, -3.000000000000095479 ) ) ;
#4521 = EDGE_CURVE ( 'NONE', #4770, #7318, #1327, .T. ) ;
#4522 = PRESENTATION_STYLE_ASSIGNMENT (( #6585 ) ) ;
#4523 = CARTESIAN_POINT ( 'NONE',  ( 1.714606436958001585E-17, 2.999951001679301835E-15, -3.000000000000000888 ) ) ;
#4524 = CARTESIAN_POINT ( 'NONE',  ( 5.790006757277029514, -62.30949558554882373, -1.494673596136803839 ) ) ;
#4525 = CARTESIAN_POINT ( 'NONE',  ( -1.424128410011220147, -67.64226375110297340, -1.734372748508781870 ) ) ;
#4526 = CARTESIAN_POINT ( 'NONE',  ( -14.18459254737392072, -36.69969775685165558, -0.4662714048949997969 ) ) ;
#4527 = CARTESIAN_POINT ( 'NONE',  ( -6.239404450008960268, -62.05055862403510503, 1.429382062327010150 ) ) ;
#4528 = FACE_OUTER_BOUND ( 'NONE', #4630, .T. ) ;
#4529 = CYLINDRICAL_SURFACE ( 'NONE', #4088, 147.0000000000000000 ) ;
#4530 = CARTESIAN_POINT ( 'NONE',  ( -28.22553731214382111, -35.79092421365019305, -3.000000000000036859 ) ) ;
#4531 = ORIENTED_EDGE ( 'NONE', *, *, #3426, .T. ) ;
#4532 = EDGE_CURVE ( 'NONE', #5341, #6990, #684, .T. ) ;
#4533 = DIRECTION ( 'NONE',  ( 5.715354789845005112E-18, 9.999836672264339449E-16, -1.000000000000000000 ) ) ;
#4534 = FACE_OUTER_BOUND ( 'NONE', #2159, .T. ) ;
#4535 = CARTESIAN_POINT ( 'NONE',  ( 13.19545720709724890, -35.82600185752891520, -3.556183125752454544E-14 ) ) ;
#4536 = CARTESIAN_POINT ( 'NONE',  ( 3.575547067216904740, -66.56692562923595347, -0.8973241761454349152 ) ) ;
#4537 = CARTESIAN_POINT ( 'NONE',  ( -16.51707533432788111, -40.85914143033993895, -4.095287503286137508E-14 ) ) ;
#4538 = ORIENTED_EDGE ( 'NONE', *, *, #1818, .T. ) ;
#4539 = EDGE_CURVE ( 'NONE', #937, #1893, #3545, .T. ) ;
#4540 = EDGE_CURVE ( 'NONE', #3706, #7067, #4874, .T. ) ;
#4541 = DIRECTION ( 'NONE',  ( -0.4950421911735701785, 0.8688689365825380539, 8.660254037844390366E-16 ) ) ;
#4542 = CARTESIAN_POINT ( 'NONE',  ( 5.193956696153660069, -59.28518064773341933, 2.254869812567109832 ) ) ;
#4543 = DIRECTION ( 'NONE',  ( -1.602374898470634869E-16, 1.442524254523139935E-17, 1.000000000000000000 ) ) ;
#4544 = DIRECTION ( 'NONE',  ( -5.715354789845005112E-18, -9.999836672264339449E-16, 1.000000000000000000 ) ) ;
#4545 = CARTESIAN_POINT ( 'NONE',  ( -4.957894848432390589, -59.36360895465049481, -1.768545648133530879 ) ) ;
#4546 = CARTESIAN_POINT ( 'NONE',  ( 27.31013720395375799, -34.44420721133294450, 3.877994099121481852 ) ) ;
#4547 = CARTESIAN_POINT ( 'NONE',  ( -2.865380587567759374, -66.05540079135724341, -0.9521156314410413879 ) ) ;
#4548 = VERTEX_POINT ( 'NONE', #6446 ) ;
#4549 = EDGE_CURVE ( 'NONE', #6356, #354, #2286, .T. ) ;
#4550 = VERTEX_POINT ( 'NONE', #2633 ) ;
#4551 = ORIENTED_EDGE ( 'NONE', *, *, #6011, .T. ) ;
#4552 = DIRECTION ( 'NONE',  ( -0.9999836672264332815, 0.005715354789845002517, 0.000000000000000000 ) ) ;
#4553 = ORIENTED_EDGE ( 'NONE', *, *, #1501, .F. ) ;
#4554 = DIRECTION ( 'NONE',  ( 0.000000000000000000, 1.000000000000000000, 1.734723475976805517E-15 ) ) ;
#4555 = FACE_OUTER_BOUND ( 'NONE', #3075, .T. ) ;
#4556 = CYLINDRICAL_SURFACE ( 'NONE', #6661, 5.000000000000000000 ) ;
#4557 = CARTESIAN_POINT ( 'NONE',  ( -6.268616217933410617, -56.62827303305337523, 1.003072567477500066 ) ) ;
#4558 = ORIENTED_EDGE ( 'NONE', *, *, #3107, .T. ) ;
#4559 = EDGE_CURVE ( 'NONE', #1044, #4778, #496, .T. ) ;
#4560 = ORIENTED_EDGE ( 'NONE', *, *, #4294, .F. ) ;
#4561 = DIRECTION ( 'NONE',  ( -5.715354789860003484E-18, -9.999836672264337477E-16, 1.000000000000000000 ) ) ;
#4562 = DIRECTION ( 'NONE',  ( 5.715354789845005112E-18, 9.999836672264339449E-16, -1.000000000000000000 ) ) ;
#4563 = CARTESIAN_POINT ( 'NONE',  ( 14.63763862841553376, 20.11382921380833011, -2.993845543551509447 ) ) ;
#4564 = DIRECTION ( 'NONE',  ( 0.7411265327553895332, 0.6713653717953992350, 6.755902076156661002E-16 ) ) ;
#4565 = FACE_OUTER_BOUND ( 'NONE', #952, .T. ) ;
#4566 = DIRECTION ( 'NONE',  ( -0.9283625964242117057, 0.005306008274017372239, 0.3716379095795966370 ) ) ;
#4567 = ORIENTED_EDGE ( 'NONE', *, *, #669, .T. ) ;
#4568 = CARTESIAN_POINT ( 'NONE',  ( 18.63446967293817735, -39.96588886641734462, 3.999999999999968026 ) ) ;
#4569 = PLANE ( 'NONE',  #2688 ) ;
#4570 = EDGE_CURVE ( 'NONE', #507, #2611, #7335, .T. ) ;
#4571 = DIRECTION ( 'NONE',  ( 0.9999836672264332815, -0.005715354789859975783, 0.000000000000000000 ) ) ;
#4572 = CARTESIAN_POINT ( 'NONE',  ( -3.381846796090564933, -54.21055914560344746, 0.1632119451740500493 ) ) ;
#4573 = CARTESIAN_POINT ( 'NONE',  ( 15.01043771185145381, 6.851040774847841242, 3.000000000000007105 ) ) ;
#4574 = ORIENTED_EDGE ( 'NONE', *, *, #3271, .F. ) ;
#4575 = CARTESIAN_POINT ( 'NONE',  ( 18.74668230531430169, -39.89873697698325117, 3.999999999999960032 ) ) ;
#4576 = DIRECTION ( 'NONE',  ( -0.8688689365825379429, -0.4950421911735701230, -5.000000000000004333E-16 ) ) ;
#4577 = VECTOR ( 'NONE', #5822, 1000.000000000000114 ) ;
#4578 = APPLICATION_CONTEXT ( 'automotive_design' ) ;
#4579 = DIRECTION ( 'NONE',  ( 2.857391495672265093E-16, 4.793132013414519254E-17, 1.000000000000000000 ) ) ;
#4580 = EDGE_CURVE ( 'NONE', #1914, #4962, #975, .T. ) ;
#4581 = CARTESIAN_POINT ( 'NONE',  ( -5.725946002089390419, -61.92844332740136792, 1.548851071596535123 ) ) ;
#4582 = LINE ( 'NONE', #2870, #271 ) ;
#4583 = DIRECTION ( 'NONE',  ( 0.3144066910790610514, 0.9492883822130742111, 0.000000000000000000 ) ) ;
#4584 = ORIENTED_EDGE ( 'NONE', *, *, #3504, .T. ) ;
#4585 = VERTEX_POINT ( 'NONE', #1545 ) ;
#4586 = ORIENTED_EDGE ( 'NONE', *, *, #6120, .F. ) ;
#4587 = AXIS2_PLACEMENT_3D ( 'NONE', #6754, #3895, #3969 ) ;
#4588 = APPLICATION_PROTOCOL_DEFINITION ( 'draft international standard', 'automotive_design', 1998, #6027 ) ;
#4589 = CARTESIAN_POINT ( 'NONE',  ( -32.93157973858376408, 14.54341967768581512, 1.435496648130876646E-14 ) ) ;
#4590 = ORIENTED_EDGE ( 'NONE', *, *, #1458, .F. ) ;
#4591 = DIRECTION ( 'NONE',  ( 0.9999836672264332815, -0.005715354789859936752, 0.000000000000000000 ) ) ;
#4592 = EDGE_CURVE ( 'NONE', #3589, #3333, #7299, .T. ) ;
#4593 = EDGE_CURVE ( 'NONE', #4811, #7283, #2, .T. ) ;
#4594 = CARTESIAN_POINT ( 'NONE',  ( -44.78727511552453677, -94.39397278840091587, -3.001000000000095813 ) ) ;
#4595 = AXIS2_PLACEMENT_3D ( 'NONE', #4537, #2785, #5559 ) ;
#4596 = CARTESIAN_POINT ( 'NONE',  ( -11.40395268922818062, 1.749910050107414738, 1.734723475976807094E-15 ) ) ;
#4597 = CARTESIAN_POINT ( 'NONE',  ( -6.733769393910259637, -61.90091566649680743, 1.831080987178660191 ) ) ;
#4598 = VERTEX_POINT ( 'NONE', #4979 ) ;
#4599 = ORIENTED_EDGE ( 'NONE', *, *, #2695, .T. ) ;
#4600 = DIRECTION ( 'NONE',  ( 0.3144066910790611624, 0.9492883822130744331, 6.800116025829053242E-16 ) ) ;
#4601 = DIRECTION ( 'NONE',  ( -0.3144066910790611624, -0.9492883822130743221, 0.000000000000000000 ) ) ;
#4602 = EDGE_CURVE ( 'NONE', #3922, #4023, #5015, .T. ) ;
#4603 = FACE_OUTER_BOUND ( 'NONE', #304, .T. ) ;
#4604 = CARTESIAN_POINT ( 'NONE',  ( 27.99155020439383890, -34.64269665048639979, 2.999999999999965805 ) ) ;
#4605 = CARTESIAN_POINT ( 'NONE',  ( -0.2323920193587202254, -101.5535681745463279, -1.014813233446432150E-13 ) ) ;
#4606 = CIRCLE ( 'NONE', #1586, 1.000000000000000000 ) ;
#4607 = ORIENTED_EDGE ( 'NONE', *, *, #3098, .F. ) ;
#4608 = AXIS2_PLACEMENT_3D ( 'NONE', #789, #2162, #7322 ) ;
#4609 = DIRECTION ( 'NONE',  ( 0.3144066910790611624, 0.9492883822130744331, 0.000000000000000000 ) ) ;
#4610 = VECTOR ( 'NONE', #6287, 1000.000000000000000 ) ;
#4611 = DIRECTION ( 'NONE',  ( 0.9999836672264332815, -0.005715354789860000936, 0.000000000000000000 ) ) ;
#4612 = DIRECTION ( 'NONE',  ( -5.715354789860003484E-18, -9.999836672264337477E-16, 1.000000000000000000 ) ) ;
#4613 = CARTESIAN_POINT ( 'NONE',  ( -6.626722312431940765, -62.23055248060769884, 1.814117920127710226 ) ) ;
#4614 = DIRECTION ( 'NONE',  ( 5.715354789860003484E-18, 9.999836672264337477E-16, -1.000000000000000000 ) ) ;
#4615 = VECTOR ( 'NONE', #1443, 1000.000000000000000 ) ;
#4616 = AXIS2_PLACEMENT_3D ( 'NONE', #3699, #730, #100 ) ;
#4617 = ORIENTED_EDGE ( 'NONE', *, *, #5886, .F. ) ;
#4618 = AXIS2_PLACEMENT_3D ( 'NONE', #1770, #4063, #6365 ) ;
#4619 = CARTESIAN_POINT ( 'NONE',  ( 9.311407240687648468, -51.41373841511902043, -1.502481404894999928 ) ) ;
#4620 = CYLINDRICAL_SURFACE ( 'NONE', #2315, 1.100000000000000755 ) ;
#4621 = CARTESIAN_POINT ( 'NONE',  ( -17.02208700381124729, 2.051506657828176650, 2.168404344971008868E-15 ) ) ;
#4622 = VECTOR ( 'NONE', #7050, 1000.000000000000114 ) ;
#4623 = AXIS2_PLACEMENT_3D ( 'NONE', #805, #2537, #177 ) ;
#4624 = CARTESIAN_POINT ( 'NONE',  ( -14.49899450467539985, -35.75040780681265318, -2.566271404894997499 ) ) ;
#4625 = CARTESIAN_POINT ( 'NONE',  ( -1.449391072403324099, -66.17791180637956927, 1.195139069250764852 ) ) ;
#4626 = AXIS2_PLACEMENT_3D ( 'NONE', #2209, #5650, #6840 ) ;
#4627 = CARTESIAN_POINT ( 'NONE',  ( 26.87031364676134970, -34.69479876584121314, 3.999999999999965361 ) ) ;
#4628 = CYLINDRICAL_SURFACE ( 'NONE', #3245, 0.9999999999999980016 ) ;
#4629 = VERTEX_POINT ( 'NONE', #5550 ) ;
#4630 = EDGE_LOOP ( 'NONE', ( #1302, #687, #938 ) ) ;
#4631 = ORIENTED_EDGE ( 'NONE', *, *, #6843, .T. ) ;
#4632 = EDGE_CURVE ( 'NONE', #6609, #6505, #5659, .T. ) ;
#4633 = AXIS2_PLACEMENT_3D ( 'NONE', #2457, #7049, #6007 ) ;
#4634 = AXIS2_PLACEMENT_3D ( 'NONE', #2304, #1786, #1189 ) ;
#4635 = APPLICATION_PROTOCOL_DEFINITION ( 'draft international standard', 'automotive_design', 1998, #6777 ) ;
#4636 = DIRECTION ( 'NONE',  ( -5.715354789860003484E-18, -9.999836672264337477E-16, 1.000000000000000000 ) ) ;
#4637 = DIRECTION ( 'NONE',  ( -0.8688689365825379429, -0.4950421911735701230, -3.889776975374848285E-16 ) ) ;
#4638 = CARTESIAN_POINT ( 'NONE',  ( 3.455862201155819768, -54.25194821296495462, -1.605226101400722083 ) ) ;
#4639 = DIRECTION ( 'NONE',  ( 0.000000000000000000, -0.7252570966694443788, 0.6884781359858918037 ) ) ;
#4640 = CARTESIAN_POINT ( 'NONE',  ( 1.662636012147085118, -65.62619303409478277, -3.045852711070930141 ) ) ;
#4641 = AXIS2_PLACEMENT_3D ( 'NONE', #3382, #4564, #598 ) ;
#4642 = ORIENTED_EDGE ( 'NONE', *, *, #140, .T. ) ;
#4643 = EDGE_CURVE ( 'NONE', #4166, #5010, #5423, .T. ) ;
#4644 = EDGE_CURVE ( 'NONE', #3100, #6678, #6086, .T. ) ;
#4645 = CARTESIAN_POINT ( 'NONE',  ( 41.70778007397900211, -94.98992620957551480, -9.475926987523308753E-14 ) ) ;
#4646 = CARTESIAN_POINT ( 'NONE',  ( -12.20412794045469518, -35.68083184586667045, -3.575000000000001175E-14 ) ) ;
#4647 = DIRECTION ( 'NONE',  ( 0.9999836672264332815, -0.005715354789860036498, 0.000000000000000000 ) ) ;
#4648 = LINE ( 'NONE', #41, #5836 ) ;
#4649 = FACE_OUTER_BOUND ( 'NONE', #445, .T. ) ;
#4650 = PRESENTATION_STYLE_ASSIGNMENT (( #3427 ) ) ;
#4651 = ORIENTED_EDGE ( 'NONE', *, *, #6120, .T. ) ;
#4652 = ORIENTED_EDGE ( 'NONE', *, *, #206, .T. ) ;
#4653 = EDGE_CURVE ( 'NONE', #2542, #6227, #1512, .T. ) ;
#4654 =( NAMED_UNIT ( * ) PLANE_ANGLE_UNIT ( ) SI_UNIT ( $, .RADIAN. ) );
#4655 = CARTESIAN_POINT ( 'NONE',  ( 1.714606436958001585E-17, 2.999951001679301835E-15, -3.000000000000000888 ) ) ;
#4656 = LINE ( 'NONE', #53, #2882 ) ;
#4657 = CARTESIAN_POINT ( 'NONE',  ( 20.29543457672885154, -41.45429371584162226, 2.999999999999958700 ) ) ;
#4658 = ORIENTED_EDGE ( 'NONE', *, *, #2996, .T. ) ;
#4659 = DIRECTION ( 'NONE',  ( -5.715354789860003484E-18, -9.999836672264337477E-16, 1.000000000000000000 ) ) ;
#4660 = FILL_AREA_STYLE ('',( #2557 ) ) ;
#4661 = DIRECTION ( 'NONE',  ( -0.9147661038495505936, 0.4039838799357137744, 3.987490689252539707E-16 ) ) ;
#4662 = LINE ( 'NONE', #6238, #1485 ) ;
#4663 = CARTESIAN_POINT ( 'NONE',  ( -5.101403815575769940, -63.43555091703197490, 1.460123530859765317 ) ) ;
#4664 = DIRECTION ( 'NONE',  ( 0.9999836672264332815, -0.005715354789859183882, 0.000000000000000000 ) ) ;
#4665 = DIRECTION ( 'NONE',  ( 0.3128416502900974727, -0.9445788350777317710, 0.09950339776592416474 ) ) ;
#4666 = EDGE_LOOP ( 'NONE', ( #1312, #3251, #7220, #4822 ) ) ;
#4667 = ORIENTED_EDGE ( 'NONE', *, *, #7423, .T. ) ;
#4668 = ORIENTED_EDGE ( 'NONE', *, *, #2730, .F. ) ;
#4669 = LINE ( 'NONE', #3523, #1603 ) ;
#4670 = DIRECTION ( 'NONE',  ( 0.5894575778543340583, -0.6507077505550991070, -0.4786639607048190914 ) ) ;
#4671 = CARTESIAN_POINT ( 'NONE',  ( -1.794944750655344867, -54.19869589391355191, -2.224588173883939035 ) ) ;
#4672 = CARTESIAN_POINT ( 'NONE',  ( 27.09819939871877637, -34.56495977950342535, -0.9765397587610813446 ) ) ;
#4673 = ADVANCED_FACE ( 'NONE', ( #2104 ), #1581, .T. ) ;
#4674 = ORIENTED_EDGE ( 'NONE', *, *, #1810, .T. ) ;
#4675 = CARTESIAN_POINT ( 'NONE',  ( -11.43300101767539623, 1.239551422827351201, 3.000000000000001332 ) ) ;
#4676 = CARTESIAN_POINT ( 'NONE',  ( -14.10560172626255948, -36.93819879313630139, 2.021321650943620263 ) ) ;
#4677 = DIRECTION ( 'NONE',  ( 0.9999836672264332815, -0.005715354789859956701, 0.000000000000000000 ) ) ;
#4678 = CARTESIAN_POINT ( 'NONE',  ( 6.162074140922939591, -62.32076522084695114, 2.666565443060120444 ) ) ;
#4679 = EDGE_CURVE ( 'NONE', #5405, #3706, #5510, .T. ) ;
#4680 = EDGE_CURVE ( 'NONE', #6339, #461, #908, .T. ) ;
#4681 = DIRECTION ( 'NONE',  ( 5.715354789845005112E-18, 9.999836672264339449E-16, -1.000000000000000000 ) ) ;
#4682 = ORIENTED_EDGE ( 'NONE', *, *, #235, .T. ) ;
#4683 = CARTESIAN_POINT ( 'NONE',  ( 4.964513617332250384, -59.39532806039484569, 1.236961020452715054 ) ) ;
#4684 = CARTESIAN_POINT ( 'NONE',  ( -14.49899450467539985, -35.75040780681265318, -0.4662714048949997969 ) ) ;
#4685 = CARTESIAN_POINT ( 'NONE',  ( 4.743586762672791224, -62.02470411057556277, -2.725691114197594800 ) ) ;
#4686 = EDGE_CURVE ( 'NONE', #2204, #5783, #4940, .T. ) ;
#4687 = EDGE_CURVE ( 'NONE', #3571, #5033, #3718, .T. ) ;
#4688 = CARTESIAN_POINT ( 'NONE',  ( 1.714606436953501688E-17, 2.999951001679301835E-15, 0.000000000000000000 ) ) ;
#4689 = ORIENTED_EDGE ( 'NONE', *, *, #4072, .F. ) ;
#4690 = CARTESIAN_POINT ( 'NONE',  ( 15.04504472124806114, -38.21726078621907874, 2.999999999999961808 ) ) ;
#4691 = CARTESIAN_POINT ( 'NONE',  ( 27.25776622504945124, -34.47404582456791644, 3.261208021432587589 ) ) ;
#4692 = PLANE ( 'NONE',  #284 ) ;
#4693 = CARTESIAN_POINT ( 'NONE',  ( 5.216904734083789741, -62.90507476914316953, -1.366939949738901872 ) ) ;
#4694 = CARTESIAN_POINT ( 'NONE',  ( 2.986904076224405014, -66.15109244657664078, 2.931604786918900363 ) ) ;
#4695 = CARTESIAN_POINT ( 'NONE',  ( -14.07431766324681988, -37.03265636863024923, 1.026284428608169819 ) ) ;
#4696 = ORIENTED_EDGE ( 'NONE', *, *, #2521, .T. ) ;
#4697 = ORIENTED_EDGE ( 'NONE', *, *, #6506, .T. ) ;
#4698 = ORIENTED_EDGE ( 'NONE', *, *, #4303, .T. ) ;
#4699 = VECTOR ( 'NONE', #2107, 1000.000000000000000 ) ;
#4700 = LINE ( 'NONE', #6432, #5585 ) ;
#4701 = DIRECTION ( 'NONE',  ( 0.000000000000000000, 0.000000000000000000, -1.000000000000000000 ) ) ;
#4702 = CARTESIAN_POINT ( 'NONE',  ( -6.238986924797109701, -58.62463756020586914, -0.4569988612983747478 ) ) ;
#4703 = CARTESIAN_POINT ( 'NONE',  ( 27.31013562793543770, -34.44420810927673671, -0.8781215038714056398 ) ) ;
#4704 = CIRCLE ( 'NONE', #5303, 11.50000000000000178 ) ;
#4705 = EDGE_LOOP ( 'NONE', ( #2944, #2343, #3215, #7024 ) ) ;
#4706 = VERTEX_POINT ( 'NONE', #4942 ) ;
#4707 = EDGE_CURVE ( 'NONE', #418, #7431, #3230, .T. ) ;
#4708 = LINE ( 'NONE', #1209, #5697 ) ;
#4709 = VECTOR ( 'NONE', #1300, 1000.000000000000227 ) ;
#4710 = CARTESIAN_POINT ( 'NONE',  ( 17.88843813672055916, -40.41242482140538783, 2.999999999999959588 ) ) ;
#4711 = DIRECTION ( 'NONE',  ( 5.715354789860003484E-18, 9.999836672264337477E-16, -1.000000000000000000 ) ) ;
#4712 = DIRECTION ( 'NONE',  ( 0.9999836672264331705, -0.005715354789860001804, 0.000000000000000000 ) ) ;
#4713 = BREP_WITH_VOIDS ( 'NONE', #1460, ( #3359, #3588 ) );
#4714 = CARTESIAN_POINT ( 'NONE',  ( 6.009612259771691889, -62.32653421013910133, 2.666676400654164336 ) ) ;
#4715 = CARTESIAN_POINT ( 'NONE',  ( 4.394524616800664418, -62.98074765389134910, -0.6184872726264748488 ) ) ;
#4716 = CARTESIAN_POINT ( 'NONE',  ( 12.26605808802378661, -5.710507655519337256, -5.640309513244763609E-15 ) ) ;
#4717 = CARTESIAN_POINT ( 'NONE',  ( 3.771067679589467758, -56.05376814337366653, 0.3277224891452724109 ) ) ;
#4718 = CARTESIAN_POINT ( 'NONE',  ( 3.533549941398215211, -54.99147314093924166, 0.1611374604154752754 ) ) ;
#4719 = DIRECTION ( 'NONE',  ( 0.9999836672264331705, -0.005715354789859876036, 0.000000000000000000 ) ) ;
#4720 = ORIENTED_EDGE ( 'NONE', *, *, #2930, .T. ) ;
#4721 = CIRCLE ( 'NONE', #2176, 2.250000000000031974 ) ;
#4722 = CARTESIAN_POINT ( 'NONE',  ( -7.547756740462713054, 12.24956608134464986, 0.006154456448477074043 ) ) ;
#4723 = AXIS2_PLACEMENT_3D ( 'NONE', #4268, #970, #5931 ) ;
#4724 = EDGE_CURVE ( 'NONE', #936, #6398, #83, .T. ) ;
#4725 = CARTESIAN_POINT ( 'NONE',  ( 18.23173688611030485, -39.61666878346903076, -0.3996164340295632611 ) ) ;
#4726 = AXIS2_PLACEMENT_3D ( 'NONE', #4261, #3300, #5482 ) ;
#4727 = CARTESIAN_POINT ( 'NONE',  ( 3.371673436877395069, -65.30458424753078361, -1.190358958913985798 ) ) ;
#4728 = VECTOR ( 'NONE', #1247, 1000.000000000000000 ) ;
#4729 = CARTESIAN_POINT ( 'NONE',  ( 3.660823140336725068, -65.74644859602665292, -1.309095517728299907 ) ) ;
#4730 = CARTESIAN_POINT ( 'NONE',  ( 9.358334193258830425, -51.27205182843857045, -2.495037190209991707 ) ) ;
#4731 = VERTEX_POINT ( 'NONE', #6406 ) ;
#4732 = AXIS2_PLACEMENT_3D ( 'NONE', #6037, #4328, #1461 ) ;
#4733 = ORIENTED_EDGE ( 'NONE', *, *, #3293, .F. ) ;
#4734 = EDGE_LOOP ( 'NONE', ( #1528, #4840, #6720, #1214 ) ) ;
#4735 = AXIS2_PLACEMENT_3D ( 'NONE', #411, #5005, #4591 ) ;
#4736 = VECTOR ( 'NONE', #2425, 1000.000000000000114 ) ;
#4737 = LINE ( 'NONE', #7027, #5691 ) ;
#4738 = ORIENTED_EDGE ( 'NONE', *, *, #4559, .T. ) ;
#4739 = VECTOR ( 'NONE', #6547, 1000.000000000000227 ) ;
#4740 = FACE_OUTER_BOUND ( 'NONE', #7139, .T. ) ;
#4741 = CARTESIAN_POINT ( 'NONE',  ( 3.942295684294244928, -66.34053734621645049, -3.017350621022677259 ) ) ;
#4742 = CARTESIAN_POINT ( 'NONE',  ( 14.63724902514210058, -35.33341991383040437, 3.658178766884820465 ) ) ;
#4743 = VECTOR ( 'NONE', #6740, 1000.000000000000000 ) ;
#4744 = AXIS2_PLACEMENT_3D ( 'NONE', #4001, #3435, #5217 ) ;
#4745 = EDGE_LOOP ( 'NONE', ( #1450, #2358, #5775 ) ) ;
#4746 = VECTOR ( 'NONE', #6218, 1000.000000000000000 ) ;
#4747 = CARTESIAN_POINT ( 'NONE',  ( -14.38395162568180652, 6.352317343304402009, 3.000000000000006217 ) ) ;
#4748 = DIRECTION ( 'NONE',  ( 0.7411265327553895332, 0.6713653717953992350, 6.755902076156661002E-16 ) ) ;
#4749 = VECTOR ( 'NONE', #1175, 1000.000000000000227 ) ;
#4750 = DIRECTION ( 'NONE',  ( 0.9999836672264333925, -0.005715354789844381486, 0.000000000000000000 ) ) ;
#4751 = CARTESIAN_POINT ( 'NONE',  ( 1.700848490796859958, -66.65813550864595527, 0.8993149516912349872 ) ) ;
#4752 = CARTESIAN_POINT ( 'NONE',  ( -4.423017985506799477, -63.40237279495851652, -1.015450938335749953 ) ) ;
#4753 = CARTESIAN_POINT ( 'NONE',  ( 12.08768627091661330, 18.45115358720316223, -2.230393353321901806 ) ) ;
#4754 = LINE ( 'NONE', #118, #4929 ) ;
#4755 = CARTESIAN_POINT ( 'NONE',  ( -4.146345969758961303, -64.48517036809602132, -2.792927026443133620 ) ) ;
#4756 = ADVANCED_FACE ( 'NONE', ( #3991 ), #1656, .T. ) ;
#4757 = VERTEX_POINT ( 'NONE', #1776 ) ;
#4758 = CARTESIAN_POINT ( 'NONE',  ( 27.30483170388656333, -34.44723004512044895, -0.1320675480243696243 ) ) ;
#4759 = DIRECTION ( 'NONE',  ( -5.715354789845005112E-18, -9.999836672264339449E-16, 1.000000000000000000 ) ) ;
#4760 = CARTESIAN_POINT ( 'NONE',  ( 19.86817077757007510, -41.71399671145089627, 2.999999999999958256 ) ) ;
#4761 = CARTESIAN_POINT ( 'NONE',  ( -1.592557218785495055, -66.68601476236933934, 1.076257986235874764 ) ) ;
#4762 = CARTESIAN_POINT ( 'NONE',  ( -4.892892059336399591, -61.27075929137718191, 2.302341147961269652 ) ) ;
#4763 = DIRECTION ( 'NONE',  ( 0.9999836672264332815, -0.005715354789859975783, 0.000000000000000000 ) ) ;
#4764 = EDGE_CURVE ( 'NONE', #6339, #5766, #6263, .T. ) ;
#4765 = CARTESIAN_POINT ( 'NONE',  ( -27.61161960580294661, 13.06853103689918427, -1.493845543551522104 ) ) ;
#4766 = ORIENTED_EDGE ( 'NONE', *, *, #343, .T. ) ;
#4767 = EDGE_CURVE ( 'NONE', #2618, #2328, #715, .T. ) ;
#4768 = VERTEX_POINT ( 'NONE', #1178 ) ;
#4769 = ORIENTED_EDGE ( 'NONE', *, *, #1940, .F. ) ;
#4770 = VERTEX_POINT ( 'NONE', #1808 ) ;
#4771 = PRODUCT ( 'Pivot Pin Rivet', 'Pivot Pin Rivet', '', ( #2011 ) ) ;
#4772 = CARTESIAN_POINT ( 'NONE',  ( 6.643375263299909683, -62.64442119333418901, -2.502572238011808281 ) ) ;
#4773 = CARTESIAN_POINT ( 'NONE',  ( -16.51707533432788111, -40.85914143033993895, -4.095287503286137508E-14 ) ) ;
#4774 = CARTESIAN_POINT ( 'NONE',  ( 3.575547067216904740, -66.56692562923595347, -0.8973241761454349152 ) ) ;
#4775 = DIRECTION ( 'NONE',  ( 5.715354789845005112E-18, 9.999836672264339449E-16, -1.000000000000000000 ) ) ;
#4776 = ORIENTED_EDGE ( 'NONE', *, *, #5131, .F. ) ;
#4777 = ADVANCED_FACE ( 'NONE', ( #5136 ), #3606, .F. ) ;
#4778 = VERTEX_POINT ( 'NONE', #4069 ) ;
#4779 = EDGE_LOOP ( 'NONE', ( #6574, #7367, #756, #4586, #5165, #570 ) ) ;
#4780 = SHAPE_REPRESENTATION_RELATIONSHIP ( 'NONE' , 'NONE' ,  #5284, #1803 ) ;
#4781 = FACE_OUTER_BOUND ( 'NONE', #4745, .T. ) ;
#4782 = CARTESIAN_POINT ( 'NONE',  ( 9.290270525626649345, 17.28063226168697497, 2.735643510310428628 ) ) ;
#4783 = LINE ( 'NONE', #4858, #4739 ) ;
#4784 = CARTESIAN_POINT ( 'NONE',  ( -32.93157973858376408, 14.54341967768581867, -2.999999999999986677 ) ) ;
#4785 = ORIENTED_EDGE ( 'NONE', *, *, #2444, .T. ) ;
#4786 = ORIENTED_EDGE ( 'NONE', *, *, #5148, .T. ) ;
#4787 = CARTESIAN_POINT ( 'NONE',  ( 27.30483170388682979, -34.44723004512030684, 2.999999999999965805 ) ) ;
#4788 = CARTESIAN_POINT ( 'NONE',  ( 4.514859508800350696, -57.62591736726079006, 0.04509635899271501047 ) ) ;
#4789 = FACE_OUTER_BOUND ( 'NONE', #5504, .T. ) ;
#4790 = CARTESIAN_POINT ( 'NONE',  ( -8.617355793880991044, 7.615193964809151339, 7.565818341857973962E-15 ) ) ;
#4791 = CARTESIAN_POINT ( 'NONE',  ( -3.433631738237976183, -65.10219846222973672, -0.7473139100181247496 ) ) ;
#4792 = CARTESIAN_POINT ( 'NONE',  ( -6.272953878096410030, -61.45586155529391448, 1.493064301322690968 ) ) ;
#4793 = EDGE_LOOP ( 'NONE', ( #4900, #899, #2366, #2517 ) ) ;
#4794 = LINE ( 'NONE', #3579, #1114 ) ;
#4795 = EDGE_CURVE ( 'NONE', #6066, #364, #2853, .T. ) ;
#4796 = CARTESIAN_POINT ( 'NONE',  ( -13.60410507457170226, -35.67283034916086848, -3.575000000000001175E-14 ) ) ;
#4797 = DIRECTION ( 'NONE',  ( 0.9492883822130744331, -0.3144066910790611624, 0.000000000000000000 ) ) ;
#4798 = CARTESIAN_POINT ( 'NONE',  ( 18.15155958994787611, -39.66235017763963810, -0.3073999163891736330 ) ) ;
#4799 = CARTESIAN_POINT ( 'NONE',  ( -5.354034084503060065, -64.02545556441495478, -0.7792797212839647214 ) ) ;
#4800 = DIRECTION ( 'NONE',  ( -5.715354789860003484E-18, -9.999836672264337477E-16, 1.000000000000000000 ) ) ;
#4801 = FACE_OUTER_BOUND ( 'NONE', #2954, .T. ) ;
#4802 = ORIENTED_EDGE ( 'NONE', *, *, #5590, .T. ) ;
#4803 = ORIENTED_EDGE ( 'NONE', *, *, #1546, .F. ) ;
#4804 = ORIENTED_EDGE ( 'NONE', *, *, #6257, .F. ) ;
#4805 = EDGE_CURVE ( 'NONE', #6323, #5266, #2293, .T. ) ;
#4806 = DIRECTION ( 'NONE',  ( -0.9828140593167951078, 0.1845982795403117438, 1.789781334969680744E-16 ) ) ;
#4807 = AXIS2_PLACEMENT_3D ( 'NONE', #711, #2973, #3080 ) ;
#4808 = CARTESIAN_POINT ( 'NONE',  ( -41.31559769795914150, -94.79889909491285493, -3.001000000000096257 ) ) ;
#4809 = CARTESIAN_POINT ( 'NONE',  ( -4.797760869400969241, -62.71499483963494015, 1.636667228454699696 ) ) ;
#4810 = ORIENTED_EDGE ( 'NONE', *, *, #6555, .F. ) ;
#4811 = VERTEX_POINT ( 'NONE', #6301 ) ;
#4812 = VERTEX_POINT ( 'NONE', #5251 ) ;
#4813 = ORIENTED_EDGE ( 'NONE', *, *, #2036, .T. ) ;
#4814 = VECTOR ( 'NONE', #6996, 1000.000000000000114 ) ;
#4815 = EDGE_CURVE ( 'NONE', #3922, #212, #2258, .T. ) ;
#4816 = EDGE_CURVE ( 'NONE', #5972, #5703, #3462, .T. ) ;
#4817 = LINE ( 'NONE', #7036, #5212 ) ;
#4818 = DIRECTION ( 'NONE',  ( 0.000000000000000000, 0.000000000000000000, -1.000000000000000000 ) ) ;
#4819 = AXIS2_PLACEMENT_3D ( 'NONE', #2740, #6226, #1060 ) ;
#4820 = CARTESIAN_POINT ( 'NONE',  ( 5.361387189091391114, -62.18179348072126089, -1.559119044556545264 ) ) ;
#4821 = CARTESIAN_POINT ( 'NONE',  ( -6.634274853075190492, -62.58082626503517787, -0.8104611758546799161 ) ) ;
#4822 = ORIENTED_EDGE ( 'NONE', *, *, #676, .T. ) ;
#4823 = AXIS2_PLACEMENT_3D ( 'NONE', #6868, #5116, #2726 ) ;
#4824 = DIRECTION ( 'NONE',  ( -5.715354789860003484E-18, -9.999836672264337477E-16, 1.000000000000000000 ) ) ;
#4825 = CARTESIAN_POINT ( 'NONE',  ( -1.449391072403324099, -66.17791180637956927, 1.195139069250764852 ) ) ;
#4826 = LINE ( 'NONE', #7362, #1242 ) ;
#4827 = CARTESIAN_POINT ( 'NONE',  ( -4.418648243523263019, 30.02574454609010601, 2.992397996059992238E-14 ) ) ;
#4828 = CARTESIAN_POINT ( 'NONE',  ( 3.369499982158394413, -65.21487972265850885, -3.264809282300078941 ) ) ;
#4829 = ORIENTED_EDGE ( 'NONE', *, *, #6959, .T. ) ;
#4830 = CARTESIAN_POINT ( 'NONE',  ( 13.14859132361180194, 19.41219719266456423, 0.4060579846640096635 ) ) ;
#4831 = AXIS2_PLACEMENT_3D ( 'NONE', #5602, #4459, #3207 ) ;
#4832 = CARTESIAN_POINT ( 'NONE',  ( 26.98506203061672792, -34.62942033074510562, 3.499999999999965361 ) ) ;
#4833 = LINE ( 'NONE', #5934, #1495 ) ;
#4834 = CARTESIAN_POINT ( 'NONE',  ( 18.06060404229330985, -40.30936335904925727, -0.6147998435448814858 ) ) ;
#4835 = CARTESIAN_POINT ( 'NONE',  ( -3.749938752099124972, 0.02143258046197846906, -3.000000000000000888 ) ) ;
#4836 = CARTESIAN_POINT ( 'NONE',  ( 6.411082221499690093, -62.51743072077169217, -1.649542549651403789 ) ) ;
#4837 = CARTESIAN_POINT ( 'NONE',  ( -28.26870112771624832, 11.60963389179610594, -1.499999999999988898 ) ) ;
#4838 = CIRCLE ( 'NONE', #1952, 5.000000000000001776 ) ;
#4839 = AXIS2_PLACEMENT_3D ( 'NONE', #492, #3947, #2214 ) ;
#4840 = ORIENTED_EDGE ( 'NONE', *, *, #3091, .T. ) ;
#4841 = VERTEX_POINT ( 'NONE', #2341 ) ;
#4842 = VERTEX_POINT ( 'NONE', #6852 ) ;
#4843 = DIRECTION ( 'NONE',  ( -0.005715354789845003385, -0.9999836672264335036, -1.000000000000000472E-15 ) ) ;
#4844 = CIRCLE ( 'NONE', #1469, 2.999999999999999556 ) ;
#4845 = DIRECTION ( 'NONE',  ( 0.9999836672264335036, -0.005715354789845041548, 0.000000000000000000 ) ) ;
#4846 = CARTESIAN_POINT ( 'NONE',  ( -2.818432829560444830, -65.09919931551695527, -0.6601304211325950133 ) ) ;
#4847 = CARTESIAN_POINT ( 'NONE',  ( 5.838403032797286230, -57.93839583847110219, 2.430643543276013840 ) ) ;
#4848 = EDGE_LOOP ( 'NONE', ( #1792, #1494, #373, #832 ) ) ;
#4849 = EDGE_CURVE ( 'NONE', #3970, #74, #3495, .T. ) ;
#4850 = CIRCLE ( 'NONE', #1601, 11.50000000000000178 ) ;
#4851 = EDGE_LOOP ( 'NONE', ( #291, #4111, #843, #4095 ) ) ;
#4852 = VERTEX_POINT ( 'NONE', #645 ) ;
#4853 = SHAPE_DEFINITION_REPRESENTATION ( #2410, #3195 ) ;
#4854 = CARTESIAN_POINT ( 'NONE',  ( 30.52077159997899969, 5.488396937354000471, -1.500000000001999956 ) ) ;
#4855 = AXIS2_PLACEMENT_3D ( 'NONE', #1157, #6914, #1787 ) ;
#4856 = LINE ( 'NONE', #6693, #7385 ) ;
#4857 = VECTOR ( 'NONE', #3964, 1000.000000000000114 ) ;
#4858 = CARTESIAN_POINT ( 'NONE',  ( 8.602313654423408451, 24.43087576540405337, 0.4060579846640144375 ) ) ;
#4859 = CARTESIAN_POINT ( 'NONE',  ( -6.752862897928530117, -62.17267392066884213, 1.309913053057485177 ) ) ;
#4860 = ORIENTED_EDGE ( 'NONE', *, *, #7284, .T. ) ;
#4861 = AXIS2_PLACEMENT_3D ( 'NONE', #5022, #6710, #7421 ) ;
#4862 = CIRCLE ( 'NONE', #4131, 3.250000000000000888 ) ;
#4863 = ORIENTED_EDGE ( 'NONE', *, *, #4449, .F. ) ;
#4864 = EDGE_CURVE ( 'NONE', #2388, #2243, #1142, .T. ) ;
#4865 = ORIENTED_EDGE ( 'NONE', *, *, #2646, .T. ) ;
#4866 = CYLINDRICAL_SURFACE ( 'NONE', #394, 3.750000000000000444 ) ;
#4867 = CARTESIAN_POINT ( 'NONE',  ( -5.076816837522959425, -57.40733507789485657, 1.813788655352380541 ) ) ;
#4868 = AXIS2_PLACEMENT_3D ( 'NONE', #1804, #4748, #4100 ) ;
#4869 = DIRECTION ( 'NONE',  ( 0.2223157560262044585, -0.6712493609847989262, 0.7071067811865449082 ) ) ;
#4870 = CARTESIAN_POINT ( 'NONE',  ( 94.42889356597736139, -103.2882618349535591, -3.000000000000103917 ) ) ;
#4871 = CARTESIAN_POINT ( 'NONE',  ( 3.485917318579867974, -55.75437092160269259, -1.796392032914925441 ) ) ;
#4872 = EDGE_CURVE ( 'NONE', #232, #2665, #4414, .T. ) ;
#4873 = AXIS2_PLACEMENT_3D ( 'NONE', #1388, #3184, #5509 ) ;
#4874 = B_SPLINE_CURVE_WITH_KNOTS ( 'NONE', 3,
 ( #574, #1184, #1781, #5174, #6, #5860, #3466, #2297, #5779, #121, #6374, #1220, #3502, #653, #2941, #1813, #2974, #2408, #4717, #7005, #1849, #6002, #1912, #6476, #6514, #4299, #2563, #5318, #753, #2451, #3115, #6041, #5927, #5432, #5890, #1294, #4791, #195, #1881, #5971, #7111, #231, #267, #3004, #791, #7075, #1325, #7188, #4221, #6587, #5484, #820, #4871, #7153, #2599, #3655, #4265, #1396, #1364, #3048, #4907, #1990, #3081, #3610, #5394, #1426, #3717, #153, #5363, #4755, #861, #3159, #2487, #309, #712, #3576, #2523, #4828, #4185, #1949, #6557 ),
 .UNSPECIFIED., .F., .F.,
 ( 4, 2, 1, 2, 2, 2, 2, 2, 1, 2, 2, 2, 2, 2, 2, 1, 2, 2, 2, 2, 2, 2, 1, 2, 2, 2, 2, 1, 2, 2, 2, 2, 2, 2, 1, 2, 2, 2, 2, 2, 2, 1, 2, 4 ),
 ( 0.000000000000000000, 0.03124999999999918121, 0.06249999999999836242, 0.07812499999999794609, 0.09374999999999754363, 0.1249999999999967804, 0.1562499999999960032, 0.1874999999999954758, 0.2187499999999949207, 0.2343749999999947820, 0.2499999999999946154, 0.2812499999999942268, 0.2968749999999940603, 0.3124999999999938383, 0.3437499999999935052, 0.3749999999999931166, 0.3906249999999930611, 0.4062499999999929501, 0.4374999999999928391, 0.4531249999999930056, 0.4687499999999931721, 0.4999999999999934497, 0.5312499999999937828, 0.5468749999999937828, 0.5624999999999937828, 0.5937499999999940048, 0.6093749999999940048, 0.6249999999999940048, 0.6562499999999944489, 0.6874999999999948930, 0.7031249999999950040, 0.7187499999999951150, 0.7499999999999955591, 0.7656249999999956701, 0.7812499999999958922, 0.8124999999999960032, 0.8437499999999962252, 0.8593749999999965583, 0.8749999999999968914, 0.9062499999999977796, 0.9218749999999981126, 0.9374999999999985567, 0.9687499999999992228, 1.000000000000000000 ),
 .UNSPECIFIED. ) ;
#4875 = EDGE_LOOP ( 'NONE', ( #5037, #4390, #4668 ) ) ;
#4876 = CARTESIAN_POINT ( 'NONE',  ( 26.87031364676133194, -34.69479876584122024, -0.5000000000000345279 ) ) ;
#4877 = DIRECTION ( 'NONE',  ( -0.9999836672264335036, 0.005715354789845008589, 0.000000000000000000 ) ) ;
#4878 = DIRECTION ( 'NONE',  ( 0.9879743132267128081, 0.1546180985661290141, 1.602621969470799848E-16 ) ) ;
#4879 = PRODUCT_DEFINITION_CONTEXT ( 'detailed design', #6777, 'design' ) ;
#4880 = CARTESIAN_POINT ( 'NONE',  ( -1.892846266465454841, -54.28526762408564110, -0.1610563749503846620 ) ) ;
#4881 = CARTESIAN_POINT ( 'NONE',  ( 6.135463341229070444, -63.36916140199613778, -1.604994752452352014 ) ) ;
#4882 = DIRECTION ( 'NONE',  ( -0.3144019573014847913, 0.9492899500389727629, 0.000000000000000000 ) ) ;
#4883 = VERTEX_POINT ( 'NONE', #3291 ) ;
#4884 = ORIENTED_EDGE ( 'NONE', *, *, #6734, .T. ) ;
#4885 = ORIENTED_EDGE ( 'NONE', *, *, #2504, .F. ) ;
#4886 = PLANE ( 'NONE',  #2547 ) ;
#4887 = DIRECTION ( 'NONE',  ( -0.8688689365825379429, -0.4950421911735701230, -5.000000000000004333E-16 ) ) ;
#4888 = CARTESIAN_POINT ( 'NONE',  ( -4.780177894917470027, -57.84320307688069107, -2.250545046436859931 ) ) ;
#4889 = CARTESIAN_POINT ( 'NONE',  ( -40.65229780501017842, -93.90085982332455217, -3.001000000000095369 ) ) ;
#4890 = CARTESIAN_POINT ( 'NONE',  ( 0.9559744929575736405, -54.27280436806401553, -0.007946376159375018178 ) ) ;
#4891 = ORIENTED_EDGE ( 'NONE', *, *, #7247, .T. ) ;
#4892 = ORIENTED_EDGE ( 'NONE', *, *, #6192, .F. ) ;
#4893 = ORIENTED_EDGE ( 'NONE', *, *, #910, .F. ) ;
#4894 = VERTEX_POINT ( 'NONE', #2755 ) ;
#4895 = DIRECTION ( 'NONE',  ( 1.000000000000000000, 0.000000000000000000, 0.000000000000000000 ) ) ;
#4896 = DIRECTION ( 'NONE',  ( -0.9492899500389726519, -0.3144019573014848468, 0.000000000000000000 ) ) ;
#4897 = ADVANCED_FACE ( 'NONE', ( #3328 ), #5608, .T. ) ;
#4898 = DIRECTION ( 'NONE',  ( -0.9999836672264333925, 0.005715354789860572528, 0.000000000000000000 ) ) ;
#4899 = CARTESIAN_POINT ( 'NONE',  ( -6.177752788274950113, -57.21669580536380550, -0.5454192084659099660 ) ) ;
#4900 = ORIENTED_EDGE ( 'NONE', *, *, #2556, .F. ) ;
#4901 = DIRECTION ( 'NONE',  ( -0.3144066910790607183, -0.9492883822130744331, 0.000000000000000000 ) ) ;
#4902 = CARTESIAN_POINT ( 'NONE',  ( 2.753836159791509974, -65.67748394244114252, 3.050484385245309849 ) ) ;
#4903 = ORIENTED_EDGE ( 'NONE', *, *, #1939, .F. ) ;
#4904 = EDGE_CURVE ( 'NONE', #1452, #1493, #2154, .T. ) ;
#4905 = EDGE_CURVE ( 'NONE', #5349, #1972, #2198, .T. ) ;
#4906 = CARTESIAN_POINT ( 'NONE',  ( -95.86211798318534250, -102.0316339954322018, 2.999999999999897415 ) ) ;
#4907 = CARTESIAN_POINT ( 'NONE',  ( -3.709322566982521607, -56.00042724521213700, -2.242165404915447358 ) ) ;
#4908 = VERTEX_POINT ( 'NONE', #6170 ) ;
#4909 = EDGE_CURVE ( 'NONE', #2855, #7422, #6737, .T. ) ;
#4910 = DIRECTION ( 'NONE',  ( -0.7811859829873639693, -0.4156127062761930113, 0.4658481924037536359 ) ) ;
#4911 = ADVANCED_FACE ( 'NONE', ( #1714 ), #2696, .F. ) ;
#4912 = DIRECTION ( 'NONE',  ( 0.3144066910790611624, 0.9492883822130744331, 6.800116025829053242E-16 ) ) ;
#4913 = DIRECTION ( 'NONE',  ( 0.9492899500389719858, 0.3144019573014870117, 0.000000000000000000 ) ) ;
#4914 = CARTESIAN_POINT ( 'NONE',  ( -6.216708800954390490, -58.75440211775612909, 1.606470739968075545 ) ) ;
#4915 = DIRECTION ( 'NONE',  ( 0.9999836672264332815, -0.005715354789847320975, 0.000000000000000000 ) ) ;
#4916 = CARTESIAN_POINT ( 'NONE',  ( 1.530679711083600125, -53.64394877353957014, -0.1027361406249600040 ) ) ;
#4917 = CARTESIAN_POINT ( 'NONE',  ( 14.29543924104632779, -35.83228874779774742, -3.556183125752454544E-14 ) ) ;
#4918 = ORIENTED_EDGE ( 'NONE', *, *, #4872, .F. ) ;
#4919 = ORIENTED_EDGE ( 'NONE', *, *, #5410, .T. ) ;
#4920 = EDGE_LOOP ( 'NONE', ( #7248, #7028, #5797 ) ) ;
#4921 = CARTESIAN_POINT ( 'NONE',  ( -14.49899450467539985, -35.75040780681265318, -0.4662714048949997969 ) ) ;
#4922 = ADVANCED_FACE ( 'NONE', ( #6830 ), #5070, .T. ) ;
#4923 = DIRECTION ( 'NONE',  ( 0.000000000000000000, -0.000000000000000000, 1.000000000000000000 ) ) ;
#4924 = CARTESIAN_POINT ( 'NONE',  ( -2.864422359069719981, -64.63427441546140528, 2.032225693688770374 ) ) ;
#4925 = CARTESIAN_POINT ( 'NONE',  ( -13.60410507457170226, -35.67283034916086848, -3.000000000000036415 ) ) ;
#4926 = CARTESIAN_POINT ( 'NONE',  ( -4.691628851351036467, -64.57111108347837103, 3.374496055255405746 ) ) ;
#4927 = ORIENTED_EDGE ( 'NONE', *, *, #1951, .F. ) ;
#4928 = ORIENTED_EDGE ( 'NONE', *, *, #3987, .F. ) ;
#4929 = VECTOR ( 'NONE', #5393, 1000.000000000000227 ) ;
#4930 = APPLICATION_PROTOCOL_DEFINITION ( 'draft international standard', 'automotive_design', 1998, #1111 ) ;
#4931 = CARTESIAN_POINT ( 'NONE',  ( 9.998427761233271482, -32.39925913208585939, -3.252606517456513302E-14 ) ) ;
#4932 = DIRECTION ( 'NONE',  ( 0.9999836672264332815, -0.005715354789845002517, 0.000000000000000000 ) ) ;
#4933 = LINE ( 'NONE', #6657, #3405 ) ;
#4934 = CARTESIAN_POINT ( 'NONE',  ( -6.381106047699259598, -62.60757382768967716, 3.386766328596300113 ) ) ;
#4935 = ORIENTED_EDGE ( 'NONE', *, *, #6022, .T. ) ;
#4936 = AXIS2_PLACEMENT_3D ( 'NONE', #1097, #7413, #5089 ) ;
#4937 = ORIENTED_EDGE ( 'NONE', *, *, #404, .F. ) ;
#4938 = LINE ( 'NONE', #854, #151 ) ;
#4939 = CARTESIAN_POINT ( 'NONE',  ( -6.216708800954390490, -58.75440211775612909, 1.606470739968075545 ) ) ;
#4940 = CIRCLE ( 'NONE', #6382, 147.0000000000000000 ) ;
#4941 = DIRECTION ( 'NONE',  ( 0.3144019573014844582, -0.9492899500389728740, 0.000000000000000000 ) ) ;
#4942 = CARTESIAN_POINT ( 'NONE',  ( -45.21893524706405287, -93.36435596057614816, -9.362127331984775681E-14 ) ) ;
#4943 = AXIS2_PLACEMENT_3D ( 'NONE', #2910, #5295, #3016 ) ;
#4944 = VERTEX_POINT ( 'NONE', #5031 ) ;
#4945 = DIRECTION ( 'NONE',  ( -0.9147661038495522590, 0.4039838799357101107, 0.000000000000000000 ) ) ;
#4946 = LINE ( 'NONE', #385, #1729 ) ;
#4947 = CARTESIAN_POINT ( 'NONE',  ( -12.11759654540111875, 13.15705282150456945, 1.301042606982605321E-14 ) ) ;
#4948 = DIRECTION ( 'NONE',  ( -0.005715354789845003385, -0.9999836672264335036, -1.000000000000000472E-15 ) ) ;
#4949 = CARTESIAN_POINT ( 'NONE',  ( -5.799935258789999715, -64.30794688765904255, -0.8981536636440297094 ) ) ;
#4950 = DIRECTION ( 'NONE',  ( 0.9492883822130744331, -0.3144066910790611624, 0.000000000000000000 ) ) ;
#4951 = ORIENTED_EDGE ( 'NONE', *, *, #2234, .F. ) ;
#4952 = ADVANCED_FACE ( 'NONE', ( #552 ), #6795, .T. ) ;
#4953 = ADVANCED_FACE ( 'NONE', ( #4999 ), #516, .F. ) ;
#4954 = ORIENTED_EDGE ( 'NONE', *, *, #429, .T. ) ;
#4955 = LINE ( 'NONE', #322, #5468 ) ;
#4956 = LINE ( 'NONE', #6131, #2319 ) ;
#4957 = CARTESIAN_POINT ( 'NONE',  ( -5.172139827190740391, -61.55016382346040871, 1.714186298074440007 ) ) ;
#4958 = CIRCLE ( 'NONE', #1707, 2.999999999999999556 ) ;
#4959 = CARTESIAN_POINT ( 'NONE',  ( -5.129009619570435774, -56.77828967133876858, 1.722487601996475881 ) ) ;
#4960 = CARTESIAN_POINT ( 'NONE',  ( 5.944105978113960020, -62.47685828501489169, -3.593838583070729786 ) ) ;
#4961 = ORIENTED_EDGE ( 'NONE', *, *, #4643, .T. ) ;
#4962 = VERTEX_POINT ( 'NONE', #6209 ) ;
#4963 = ORIENTED_EDGE ( 'NONE', *, *, #3042, .F. ) ;
#4964 = VECTOR ( 'NONE', #6846, 1000.000000000000000 ) ;
#4965 = DIRECTION ( 'NONE',  ( -5.715354789860003484E-18, -9.999836672264337477E-16, 1.000000000000000000 ) ) ;
#4966 = COLOUR_RGB ( '', 0.40784314, 0.44705882, 0.49803922) ;
#4967 = FACE_OUTER_BOUND ( 'NONE', #945, .T. ) ;
#4968 = CARTESIAN_POINT ( 'NONE',  ( -16.40387102536037744, 1.778486824056639826, 1.734723475976807094E-15 ) ) ;
#4969 = CARTESIAN_POINT ( 'NONE',  ( -6.708998324124310741, -61.63987295270813860, 3.437611327301279385 ) ) ;
#4970 = VECTOR ( 'NONE', #399, 1000.000000000000000 ) ;
#4971 = AXIS2_PLACEMENT_3D ( 'NONE', #6297, #3988, #1094 ) ;
#4972 = ADVANCED_FACE ( 'NONE', ( #2798 ), #7396, .T. ) ;
#4973 = CARTESIAN_POINT ( 'NONE',  ( -95.86211798318534250, -102.0316339954322018, -1.025655255171287195E-13 ) ) ;
#4974 = CIRCLE ( 'NONE', #2923, 0.5000000000000022204 ) ;
#4975 = DIRECTION ( 'NONE',  ( 0.6713653717953971256, -0.7411265327553914206, -9.593219417351524366E-16 ) ) ;
#4976 = AXIS2_PLACEMENT_3D ( 'NONE', #1285, #5306, #3900 ) ;
#4977 = AXIS2_PLACEMENT_3D ( 'NONE', #849, #6503, #1349 ) ;
#4978 = FACE_OUTER_BOUND ( 'NONE', #2507, .T. ) ;
#4979 = CARTESIAN_POINT ( 'NONE',  ( 15.39900769062488806, 3.181283097128406290, -2.999999999999997335 ) ) ;
#4980 = AXIS2_PLACEMENT_3D ( 'NONE', #3391, #5215, #1702 ) ;
#4981 = ORIENTED_EDGE ( 'NONE', *, *, #3652, .T. ) ;
#4982 = AXIS2_PLACEMENT_3D ( 'NONE', #7271, #2110, #3355 ) ;
#4983 = CIRCLE ( 'NONE', #5958, 1.000000000000000444 ) ;
#4984 = DIRECTION ( 'NONE',  ( 0.2223191033124284066, 0.6712482523644728305, 0.7071067811865466846 ) ) ;
#4985 = EDGE_CURVE ( 'NONE', #380, #1089, #6496, .T. ) ;
#4986 = CARTESIAN_POINT ( 'NONE',  ( -14.38395162568175145, 6.352317343304510366, -2.999999999999994671 ) ) ;
#4987 = AXIS2_PLACEMENT_3D ( 'NONE', #39, #3642, #739 ) ;
#4988 = LINE ( 'NONE', #5493, #1140 ) ;
#4989 = CARTESIAN_POINT ( 'NONE',  ( -7.067610632470020526, -58.47094543896879060, 0.9162228916581999227 ) ) ;
#4990 = DIRECTION ( 'NONE',  ( 0.000000000000000000, -1.000000000000000000, -9.973300763855647239E-16 ) ) ;
#4991 = ORIENTED_EDGE ( 'NONE', *, *, #3838, .F. ) ;
#4992 = CARTESIAN_POINT ( 'NONE',  ( 25.15036705625666258, 26.15624279088187265, 2.645453300864630819E-14 ) ) ;
#4993 = CARTESIAN_POINT ( 'NONE',  ( -10.41850315652351533, -32.21925899276746463, -3.000000000000032863 ) ) ;
#4994 = LINE ( 'NONE', #5604, #7120 ) ;
#4995 = EDGE_CURVE ( 'NONE', #3340, #5544, #6455, .T. ) ;
#4996 = EDGE_CURVE ( 'NONE', #327, #3172, #4338, .T. ) ;
#4997 = CARTESIAN_POINT ( 'NONE',  ( 2.303277369485650095, -64.96541665026637702, 1.677260903589945285 ) ) ;
#4998 = DIRECTION ( 'NONE',  ( -0.9147661038495481511, 0.4039838799357194921, 3.987490689252597393E-16 ) ) ;
#4999 = FACE_OUTER_BOUND ( 'NONE', #2821, .T. ) ;
#5000 = ORIENTED_EDGE ( 'NONE', *, *, #3799, .F. ) ;
#5001 = ORIENTED_EDGE ( 'NONE', *, *, #3963, .F. ) ;
#5002 = ORIENTED_EDGE ( 'NONE', *, *, #3325, .T. ) ;
#5003 = ORIENTED_EDGE ( 'NONE', *, *, #4539, .F. ) ;
#5004 = CARTESIAN_POINT ( 'NONE',  ( -28.68093632328499965, 11.79168739492699913, -1.500000000001999956 ) ) ;
#5005 = DIRECTION ( 'NONE',  ( -5.715354789860003484E-18, -9.999836672264337477E-16, 1.000000000000000000 ) ) ;
#5006 = EDGE_CURVE ( 'NONE', #3368, #4029, #5188, .T. ) ;
#5007 = DIRECTION ( 'NONE',  ( 0.000000000000000000, -0.000000000000000000, 1.000000000000000000 ) ) ;
#5008 = CARTESIAN_POINT ( 'NONE',  ( 6.378760423371060639, -64.06988568591069111, -0.05691440262071967293 ) ) ;
#5009 = ORIENTED_EDGE ( 'NONE', *, *, #5283, .F. ) ;
#5010 = VERTEX_POINT ( 'NONE', #2463 ) ;
#5011 = CARTESIAN_POINT ( 'NONE',  ( 21.92563132188826103, 21.95321433679979961, -1.493845543551513444 ) ) ;
#5012 = CARTESIAN_POINT ( 'NONE',  ( 18.49916120972750377, -39.46430250869199341, -0.5000000000000393019 ) ) ;
#5013 = CARTESIAN_POINT ( 'NONE',  ( 1.316624512147740012, -66.75104842734066324, 3.019790780136459851 ) ) ;
#5014 = DIRECTION ( 'NONE',  ( -5.715354789860003484E-18, -9.999836672264337477E-16, 1.000000000000000000 ) ) ;
#5015 = LINE ( 'NONE', #7377, #1809 ) ;
#5016 = ORIENTED_EDGE ( 'NONE', *, *, #6874, .T. ) ;
#5017 = ORIENTED_EDGE ( 'NONE', *, *, #4403, .F. ) ;
#5018 = CARTESIAN_POINT ( 'NONE',  ( -105.7473861751082040, -118.0666774205683822, 2.999999999999881428 ) ) ;
#5019 = DIRECTION ( 'NONE',  ( 1.387778780781445676E-14, 2.775557561562891351E-14, 1.000000000000000000 ) ) ;
#5020 = LINE ( 'NONE', #7304, #604 ) ;
#5021 = CARTESIAN_POINT ( 'NONE',  ( -3.941959611298590183, -54.25574829393653431, -0.9393447306324897994 ) ) ;
#5022 = CARTESIAN_POINT ( 'NONE',  ( 0.000000000000000000, 0.000000000000000000, -17.67054229618195293 ) ) ;
#5023 = ORIENTED_EDGE ( 'NONE', *, *, #5235, .T. ) ;
#5024 = CARTESIAN_POINT ( 'NONE',  ( -108.8601514936008385, -112.6033348200152915, 3.999999999999886313 ) ) ;
#5025 = PRODUCT_DEFINITION ( 'UNKNOWN', '', #5461, #5491 ) ;
#5026 = CARTESIAN_POINT ( 'NONE',  ( -4.954937549494499827, -61.85628170826059602, 3.287035460711430268 ) ) ;
#5027 = CARTESIAN_POINT ( 'NONE',  ( 35.76131148831677109, 4.835142255982173509, 5.039451867604972471E-15 ) ) ;
#5028 = CARTESIAN_POINT ( 'NONE',  ( 1.714606436953501688E-17, 2.999951001679301835E-15, 0.000000000000000000 ) ) ;
#5029 = CARTESIAN_POINT ( 'NONE',  ( -5.038070929474960380, -61.61169989543196834, 3.303768584289609844 ) ) ;
#5030 = DIRECTION ( 'NONE',  ( 0.000000000000000000, 0.000000000000000000, -1.000000000000000000 ) ) ;
#5031 = CARTESIAN_POINT ( 'NONE',  ( 14.81352433457121975, -34.80119172639020064, 2.597518595105000383 ) ) ;
#5032 = VERTEX_POINT ( 'NONE', #4765 ) ;
#5033 = VERTEX_POINT ( 'NONE', #620 ) ;
#5034 = ORIENTED_EDGE ( 'NONE', *, *, #6959, .F. ) ;
#5035 = APPLICATION_PROTOCOL_DEFINITION ( 'draft international standard', 'automotive_design', 1998, #1264 ) ;
#5036 = LINE ( 'NONE', #7320, #3037 ) ;
#5037 = ORIENTED_EDGE ( 'NONE', *, *, #6734, .F. ) ;
#5038 = DIRECTION ( 'NONE',  ( 0.4039838799357177157, 0.9147661038495489283, 9.170600743851256632E-16 ) ) ;
#5039 = PLANE ( 'NONE',  #7132 ) ;
#5040 = CARTESIAN_POINT ( 'NONE',  ( 17.61001731287966265, -39.97089645448942719, 3.999999999999960032 ) ) ;
#5041 = CARTESIAN_POINT ( 'NONE',  ( -6.841972559203830961, -62.34857902771452842, 2.832214187714990228 ) ) ;
#5042 = ORIENTED_EDGE ( 'NONE', *, *, #1269, .T. ) ;
#5043 = EDGE_CURVE ( 'NONE', #3646, #5842, #6618, .T. ) ;
#5044 = CARTESIAN_POINT ( 'NONE',  ( -15.00216760413269945, 6.625337177075936168, 6.505213034913026604E-15 ) ) ;
#5045 = EDGE_CURVE ( 'NONE', #1906, #5376, #500, .T. ) ;
#5046 = CARTESIAN_POINT ( 'NONE',  ( 14.85956812845453889, -34.66217166146590500, 2.951071985698260125 ) ) ;
#5047 = CARTESIAN_POINT ( 'NONE',  ( 5.447354608442940282, -62.18425133612383604, -1.411124226719259855 ) ) ;
#5048 = AXIS2_PLACEMENT_3D ( 'NONE', #152, #3047, #2940 ) ;
#5049 = CARTESIAN_POINT ( 'NONE',  ( 39.97800414936823188, -95.26063634933134949, -9.497611030973018842E-14 ) ) ;
#5050 = CARTESIAN_POINT ( 'NONE',  ( -5.480856739662490540, -62.25220485324549458, 1.560007870815685260 ) ) ;
#5051 = ORIENTED_EDGE ( 'NONE', *, *, #440, .F. ) ;
#5052 = B_SPLINE_CURVE_WITH_KNOTS ( 'NONE', 3,
 ( #1897, #6495, #948, #7269, #915, #6464 ),
 .UNSPECIFIED., .F., .F.,
 ( 4, 2, 4 ),
 ( 0.000000000000000000, 0.5000000000000016653, 1.000000000000000000 ),
 .UNSPECIFIED. ) ;
#5053 = ORIENTED_EDGE ( 'NONE', *, *, #4680, .F. ) ;
#5054 = EDGE_CURVE ( 'NONE', #3671, #3409, #248, .T. ) ;
#5055 = AXIS2_PLACEMENT_3D ( 'NONE', #3602, #5916, #4146 ) ;
#5056 = CARTESIAN_POINT ( 'NONE',  ( 17.63495400270750224, -39.95668865737157205, 3.269138726291231034 ) ) ;
#5057 = CARTESIAN_POINT ( 'NONE',  ( -15.08175531864075047, -33.99084820126180517, -5.041145139047909396 ) ) ;
#5058 = CARTESIAN_POINT ( 'NONE',  ( 24.99346688245966419, 26.01411140189437177, 0.006154456448490951831 ) ) ;
#5059 = CIRCLE ( 'NONE', #3369, 0.9999999999999984457 ) ;
#5060 = CARTESIAN_POINT ( 'NONE',  ( 6.251545776960879763, -56.60079747432034480, -0.4089935619396500299 ) ) ;
#5061 = DIRECTION ( 'NONE',  ( 0.6713653717953971256, -0.7411265327553914206, -8.096059920055343791E-16 ) ) ;
#5062 = VERTEX_POINT ( 'NONE', #64 ) ;
#5063 = CYLINDRICAL_SURFACE ( 'NONE', #6870, 140.0000000000000000 ) ;
#5064 = CARTESIAN_POINT ( 'NONE',  ( -4.930053471857299918, -61.64676491032937378, 0.1765652348176402209 ) ) ;
#5065 = AXIS2_PLACEMENT_3D ( 'NONE', #4695, #4665, #1791 ) ;
#5066 = CARTESIAN_POINT ( 'NONE',  ( -27.72086689141953286, 13.93665911791780410, -1.493845543551521216 ) ) ;
#5067 = CARTESIAN_POINT ( 'NONE',  ( 0.000000000000000000, 0.000000000000000000, -17.67054229618195293 ) ) ;
#5068 = CARTESIAN_POINT ( 'NONE',  ( -1.128062821581302000, -55.49617455686423284, 0.7066123397475153611 ) ) ;
#5069 = CARTESIAN_POINT ( 'NONE',  ( 27.72483002872544944, -34.20793401062830696, 3.264201108005380547 ) ) ;
#5070 = PLANE ( 'NONE',  #840 ) ;
#5071 = ORIENTED_EDGE ( 'NONE', *, *, #6598, .T. ) ;
#5072 = ORIENTED_EDGE ( 'NONE', *, *, #5701, .F. ) ;
#5073 = ORIENTED_EDGE ( 'NONE', *, *, #5147, .T. ) ;
#5074 = DIRECTION ( 'NONE',  ( 0.9492883822130744331, -0.3144066910790611624, 0.000000000000000000 ) ) ;
#5075 = AXIS2_PLACEMENT_3D ( 'NONE', #1555, #2719, #7345 ) ;
#5076 = DIRECTION ( 'NONE',  ( 5.715354789860003484E-18, 9.999836672264337477E-16, -1.000000000000000000 ) ) ;
#5077 = CARTESIAN_POINT ( 'NONE',  ( -16.40387102536037744, 1.778486824056639826, 1.734723475976807094E-15 ) ) ;
#5078 = CARTESIAN_POINT ( 'NONE',  ( -40.65229780501022816, -93.90085982332443848, -3.000000000000095035 ) ) ;
#5079 = CARTESIAN_POINT ( 'NONE',  ( -3.328771606340945155, -66.98264282425255089, -1.647280098378362867 ) ) ;
#5080 = ADVANCED_FACE ( 'NONE', ( #4122 ), #4628, .T. ) ;
#5081 = VERTEX_POINT ( 'NONE', #7019 ) ;
#5082 = AXIS2_PLACEMENT_3D ( 'NONE', #946, #272, #4269 ) ;
#5083 = CIRCLE ( 'NONE', #1829, 1.000000000000000000 ) ;
#5084 = CARTESIAN_POINT ( 'NONE',  ( -19.94212619460468261, -40.63668738334721553, -4.075000000000002200E-14 ) ) ;
#5085 = CARTESIAN_POINT ( 'NONE',  ( 18.47982041150265431, -39.47532202006953383, 2.999999999999960476 ) ) ;
#5086 = AXIS2_PLACEMENT_3D ( 'NONE', #450, #2733, #6554 ) ;
#5087 = CARTESIAN_POINT ( 'NONE',  ( 0.000000000000000000, 0.000000000000000000, 3.000000000000000000 ) ) ;
#5088 = CIRCLE ( 'NONE', #1121, 2.500000000000000000 ) ;
#5089 = DIRECTION ( 'NONE',  ( 0.4950421911735801705, -0.8688689365825322808, 0.000000000000000000 ) ) ;
#5090 = EDGE_CURVE ( 'NONE', #5010, #1273, #6980, .T. ) ;
#5091 = ADVANCED_FACE ( 'NONE', ( #18 ), #3478, .T. ) ;
#5092 = CARTESIAN_POINT ( 'NONE',  ( -5.895255198864449930, -62.39547700480248693, 1.556969243713622220 ) ) ;
#5093 = MECHANICAL_DESIGN_GEOMETRIC_PRESENTATION_REPRESENTATION (  '', ( #6412 ), #5942 ) ;
#5094 = ORIENTED_EDGE ( 'NONE', *, *, #7245, .F. ) ;
#5095 = AXIS2_PLACEMENT_3D ( 'NONE', #1341, #4132, #4280 ) ;
#5096 = TOROIDAL_SURFACE ( 'NONE', #2560, 1.500000000000000000, 1.000000000000000000 ) ;
#5097 = DIRECTION ( 'NONE',  ( -0.5818022356294096920, 0.8133302887613499399, 8.099917986277619058E-16 ) ) ;
#5098 = CARTESIAN_POINT ( 'NONE',  ( 17.95809745115200684, -39.77257614736446811, 3.810493591301452820 ) ) ;
#5099 = DIRECTION ( 'NONE',  ( 0.9793199139485100346, 0.2023178344681531293, 1.787644449902631965E-16 ) ) ;
#5100 = AXIS2_PLACEMENT_3D ( 'NONE', #6826, #3966, #7348 ) ;
#5101 = EDGE_CURVE ( 'NONE', #2020, #1170, #4084, .T. ) ;
#5102 = CARTESIAN_POINT ( 'NONE',  ( -41.31559769795914150, -94.79889909491285493, -9.503348406515855143E-14 ) ) ;
#5103 = CARTESIAN_POINT ( 'NONE',  ( -6.891320273265630014, -62.11321098440852495, -0.2797727661029551505 ) ) ;
#5104 = CARTESIAN_POINT ( 'NONE',  ( 27.55235279947361349, -34.38166451341173513, 2.999999999999965805 ) ) ;
#5105 = AXIS2_PLACEMENT_3D ( 'NONE', #3468, #6375, #5320 ) ;
#5106 = AXIS2_PLACEMENT_3D ( 'NONE', #6092, #7065, #3804 ) ;
#5107 = EDGE_LOOP ( 'NONE', ( #6303, #6478, #2127, #920 ) ) ;
#5108 = ORIENTED_EDGE ( 'NONE', *, *, #3387, .F. ) ;
#5109 = CARTESIAN_POINT ( 'NONE',  ( -1.630661209647960019, -65.50972637651682362, 2.960670344429949807 ) ) ;
#5110 = CARTESIAN_POINT ( 'NONE',  ( 25.89376920855426079, 25.02025921737413583, -2.152344182241806347 ) ) ;
#5111 = CIRCLE ( 'NONE', #4868, 0.7499999999999872324 ) ;
#5112 =( REPRESENTATION_RELATIONSHIP ('NONE','NONE', #3195, #7047 ) REPRESENTATION_RELATIONSHIP_WITH_TRANSFORMATION ( #2840 )SHAPE_REPRESENTATION_RELATIONSHIP( ) );
#5113 = FACE_OUTER_BOUND ( 'NONE', #1538, .T. ) ;
#5114 = CARTESIAN_POINT ( 'NONE',  ( 4.394524616800664418, -62.98074765389134910, -0.6184872726264748488 ) ) ;
#5115 = CARTESIAN_POINT ( 'NONE',  ( 27.96884669319430827, -34.65534042161862516, 3.261656933814885306 ) ) ;
#5116 = DIRECTION ( 'NONE',  ( -0.9180849359830441925, 0.3963837160139272453, 3.911300608320930924E-16 ) ) ;
#5117 = B_SPLINE_CURVE_WITH_KNOTS ( 'NONE', 3,
 ( #5123, #7435, #626, #5236, #6245, #69 ),
 .UNSPECIFIED., .F., .F.,
 ( 4, 2, 4 ),
 ( 0.000000000000000000, 0.0003939438732545951058, 0.0007878877465091902116 ),
 .UNSPECIFIED. ) ;
#5118 = ORIENTED_EDGE ( 'NONE', *, *, #2996, .F. ) ;
#5119 = AXIS2_PLACEMENT_3D ( 'NONE', #2512, #3220, #1978 ) ;
#5120 = ORIENTED_EDGE ( 'NONE', *, *, #2683, .T. ) ;
#5121 = EDGE_LOOP ( 'NONE', ( #3126, #3704 ) ) ;
#5122 = ITEM_DEFINED_TRANSFORMATION ( 'NONE', 'NONE', #1007,  #751 ) ;
#5123 = CARTESIAN_POINT ( 'NONE',  ( 18.06432739836606771, -39.71205113188410962, 2.999999999999960476 ) ) ;
#5124 = DIRECTION ( 'NONE',  ( -0.9999836672264332815, 0.005715354789842956411, 0.000000000000000000 ) ) ;
#5125 = CARTESIAN_POINT ( 'NONE',  ( 14.49911764349215915, -35.75048010860329839, 0.4975185951050001831 ) ) ;
#5126 = CARTESIAN_POINT ( 'NONE',  ( 15.04504472124806114, -38.21726078621907874, -3.816391647148975608E-14 ) ) ;
#5127 = CARTESIAN_POINT ( 'NONE',  ( 1.455885123031280148, -67.63619251397972221, 2.328451870335179752 ) ) ;
#5128 = VERTEX_POINT ( 'NONE', #6353 ) ;
#5129 = ORIENTED_EDGE ( 'NONE', *, *, #5090, .F. ) ;
#5130 = DIRECTION ( 'NONE',  ( 0.3144066910790611624, 0.9492883822130744331, 0.000000000000000000 ) ) ;
#5131 = EDGE_CURVE ( 'NONE', #5892, #6872, #1221, .T. ) ;
#5132 = CARTESIAN_POINT ( 'NONE',  ( 9.311407240687648468, -51.41373841511900622, -2.502481404895003259 ) ) ;
#5133 = DIRECTION ( 'NONE',  ( 0.4364886600403628525, -0.1927644473149890403, -0.8788171126619663820 ) ) ;
#5134 = CARTESIAN_POINT ( 'NONE',  ( 38.49686355599224896, -95.49243502991532750, -9.519295074422728931E-14 ) ) ;
#5135 = DIRECTION ( 'NONE',  ( -0.9999836672264335036, 0.005715354789845041548, 0.000000000000000000 ) ) ;
#5136 = FACE_OUTER_BOUND ( 'NONE', #3295, .T. ) ;
#5137 = EDGE_LOOP ( 'NONE', ( #4865, #4919, #5869, #10 ) ) ;
#5138 = EDGE_CURVE ( 'NONE', #6678, #3671, #3120, .T. ) ;
#5139 = EDGE_CURVE ( 'NONE', #878, #3729, #4098, .T. ) ;
#5140 = LINE ( 'NONE', #6411, #3994 ) ;
#5141 = DIRECTION ( 'NONE',  ( -0.4364886600403651840, 0.1927644473149899840, 0.8788171126619650497 ) ) ;
#5142 = CARTESIAN_POINT ( 'NONE',  ( 14.63724902514211834, -35.33341991383040437, 3.658178766884810251 ) ) ;
#5143 = CARTESIAN_POINT ( 'NONE',  ( -6.126235009943979293, -64.48141016635396738, -1.469515951087519978 ) ) ;
#5144 = CARTESIAN_POINT ( 'NONE',  ( -28.70619392989860330, -36.67182071578998404, -3.001000000000038082 ) ) ;
#5145 = ORIENTED_EDGE ( 'NONE', *, *, #1774, .T. ) ;
#5146 = DIRECTION ( 'NONE',  ( -1.850371707708594129E-14, -4.394632805807911095E-14, 1.000000000000000000 ) ) ;
#5147 = EDGE_CURVE ( 'NONE', #2280, #74, #1814, .T. ) ;
#5148 = EDGE_CURVE ( 'NONE', #5486, #2020, #1272, .T. ) ;
#5149 = CARTESIAN_POINT ( 'NONE',  ( 17.88843813672053429, -40.41242482140540204, -0.1320686260247052324 ) ) ;
#5150 = DIRECTION ( 'NONE',  ( 5.715354789845005112E-18, 9.999836672264339449E-16, -1.000000000000000000 ) ) ;
#5151 = CARTESIAN_POINT ( 'NONE',  ( 4.230506805399654624, -63.24565307424497007, 1.502053860026275167 ) ) ;
#5152 = CARTESIAN_POINT ( 'NONE',  ( 27.55792178321159014, -34.88417723535314252, 3.873636197071128606 ) ) ;
#5153 = CARTESIAN_POINT ( 'NONE',  ( 5.927764221498110331, -62.35749858221746678, -1.529935281190306862 ) ) ;
#5154 = ORIENTED_EDGE ( 'NONE', *, *, #3042, .T. ) ;
#5155 = ORIENTED_EDGE ( 'NONE', *, *, #1733, .T. ) ;
#5156 = ORIENTED_EDGE ( 'NONE', *, *, #6114, .F. ) ;
#5157 = ORIENTED_EDGE ( 'NONE', *, *, #5316, .F. ) ;
#5158 = CONTEXT_DEPENDENT_SHAPE_REPRESENTATION ( #5112, #3612 ) ;
#5159 = CARTESIAN_POINT ( 'NONE',  ( 43.95483829995806957, -94.87490738911687060, -9.454242944073598665E-14 ) ) ;
#5160 = ORIENTED_EDGE ( 'NONE', *, *, #1040, .T. ) ;
#5161 = CARTESIAN_POINT ( 'NONE',  ( -17.75204616238700339, 7.839753195160374055, 2.236547809770383921 ) ) ;
#5162 = CARTESIAN_POINT ( 'NONE',  ( -25.02557223580756585, -4.388903113930568090, -4.336808689942017736E-15 ) ) ;
#5163 = CARTESIAN_POINT ( 'NONE',  ( 26.92714173160467084, -34.66242069539057979, -0.4999999559301231411 ) ) ;
#5164 = CARTESIAN_POINT ( 'NONE',  ( 3.751014749966880224, -66.74975575182239140, 0.1208598729073953049 ) ) ;
#5165 = ORIENTED_EDGE ( 'NONE', *, *, #4549, .F. ) ;
#5166 = ORIENTED_EDGE ( 'NONE', *, *, #1977, .F. ) ;
#5167 = CARTESIAN_POINT ( 'NONE',  ( 27.89660656231303193, -34.69557212064219698, -0.5230190109555528100 ) ) ;
#5168 = PLANE ( 'NONE',  #4971 ) ;
#5169 = DIRECTION ( 'NONE',  ( 0.7411265327553913096, 0.6713653717953971256, 6.570922257487902105E-16 ) ) ;
#5170 = DIRECTION ( 'NONE',  ( -0.2023178344681547114, 0.9793199139485095905, 8.673617379884032514E-16 ) ) ;
#5171 = ORIENTED_EDGE ( 'NONE', *, *, #5378, .T. ) ;
#5172 = CARTESIAN_POINT ( 'NONE',  ( 17.88843813737523192, -40.41242482244771850, 3.131634423728840488 ) ) ;
#5173 = CARTESIAN_POINT ( 'NONE',  ( -17.48918432324802907, 2.257788664364643871, 3.591483327634216849 ) ) ;
#5174 = CARTESIAN_POINT ( 'NONE',  ( -3.435267632410309080, -65.16561242980966995, 1.350366576929741491 ) ) ;
#5175 = CARTESIAN_POINT ( 'NONE',  ( -4.011890603535904987, -66.29221981733677183, 1.575336318554399595 ) ) ;
#5176 = ADVANCED_FACE ( 'NONE', ( #3585, #5900, #725 ), #5332, .F. ) ;
#5177 = DIRECTION ( 'NONE',  ( 0.9999836672264332815, -0.005715354789844959149, 0.000000000000000000 ) ) ;
#5178 = CIRCLE ( 'NONE', #7083, 20.00000000000000000 ) ;
#5179 = ORIENTED_EDGE ( 'NONE', *, *, #1043, .F. ) ;
#5180 = DIRECTION ( 'NONE',  ( 0.9999836672264332815, -0.005715354789859936752, 0.000000000000000000 ) ) ;
#5181 = SURFACE_STYLE_FILL_AREA ( #4660 ) ;
#5182 = DIRECTION ( 'NONE',  ( -0.4039838799357108323, -0.9147661038495518149, -9.170600743851223106E-16 ) ) ;
#5183 = VECTOR ( 'NONE', #7265, 1000.000000000000000 ) ;
#5184 = CARTESIAN_POINT ( 'NONE',  ( 39.48483786921892857, -95.33781693134928048, -3.001370543551635794 ) ) ;
#5185 = CARTESIAN_POINT ( 'NONE',  ( -4.773669824303439668, -63.68048849998092464, 3.536592896228280214 ) ) ;
#5186 = CARTESIAN_POINT ( 'NONE',  ( 18.74668230531428748, -39.89873697698326538, -0.5000000000000397460 ) ) ;
#5187 = ADVANCED_FACE ( 'NONE', ( #2000 ), #5940, .T. ) ;
#5188 = LINE ( 'NONE', #6949, #5798 ) ;
#5189 = EDGE_CURVE ( 'NONE', #909, #1930, #5374, .T. ) ;
#5190 = EDGE_LOOP ( 'NONE', ( #4667, #1657, #21, #4951 ) ) ;
#5191 = ORIENTED_EDGE ( 'NONE', *, *, #3324, .T. ) ;
#5192 = ORIENTED_EDGE ( 'NONE', *, *, #5198, .F. ) ;
#5193 = CARTESIAN_POINT ( 'NONE',  ( -44.78727511552453677, -94.39397278840091587, -9.464840624037363205E-14 ) ) ;
#5194 = DIRECTION ( 'NONE',  ( -0.4039838799357112764, -0.9147661038495517039, -1.194615830541411051E-15 ) ) ;
#5195 = CARTESIAN_POINT ( 'NONE',  ( 3.189415849367489564, -54.78201482374456788, -1.959602550130806753 ) ) ;
#5196 = DIRECTION ( 'NONE',  ( -0.9283625964242117057, 0.005306008274017372239, 0.3716379095795966370 ) ) ;
#5197 = CARTESIAN_POINT ( 'NONE',  ( 1.340549191775572080, -65.71857943717337491, -0.9252791854465649557 ) ) ;
#5198 = EDGE_CURVE ( 'NONE', #4378, #6950, #769, .T. ) ;
#5199 = ORIENTED_EDGE ( 'NONE', *, *, #7423, .F. ) ;
#5200 = CLOSED_SHELL ( 'NONE', ( #5926, #6292, #6416 ) ) ;
#5201 = CARTESIAN_POINT ( 'NONE',  ( -20.89962323070193406, -41.21687045383659154, -3.000000000000042188 ) ) ;
#5202 = FACE_OUTER_BOUND ( 'NONE', #2001, .T. ) ;
#5203 = CARTESIAN_POINT ( 'NONE',  ( 39.48483786921892857, -95.33781693134928048, -9.519295074422728931E-14 ) ) ;
#5204 = CARTESIAN_POINT ( 'NONE',  ( 19.34585819626726533, -40.86123582061801329, -4.076600168545496672E-14 ) ) ;
#5205 = CARTESIAN_POINT ( 'NONE',  ( 12.08768627091661330, 18.45115358720316223, -2.230393353321891592 ) ) ;
#5206 = DIRECTION ( 'NONE',  ( -0.2163384215910431896, -0.07165063022625259292, 0.9736857165079894072 ) ) ;
#5207 = AXIS2_PLACEMENT_3D ( 'NONE', #4006, #3890, #1156 ) ;
#5208 = CIRCLE ( 'NONE', #6407, 2.999999999999999556 ) ;
#5209 = ORIENTED_EDGE ( 'NONE', *, *, #7227, .T. ) ;
#5210 = VERTEX_POINT ( 'NONE', #2497 ) ;
#5211 = VECTOR ( 'NONE', #5595, 1000.000000000000000 ) ;
#5212 = VECTOR ( 'NONE', #3566, 1000.000000000000000 ) ;
#5213 = DIRECTION ( 'NONE',  ( -0.005715354789845003385, -0.9999836672264335036, -1.000000000000000472E-15 ) ) ;
#5214 = VECTOR ( 'NONE', #6769, 1000.000000000000000 ) ;
#5215 = DIRECTION ( 'NONE',  ( 0.000000000000000000, 0.000000000000000000, -1.000000000000000000 ) ) ;
#5216 = FACE_OUTER_BOUND ( 'NONE', #4415, .T. ) ;
#5217 = DIRECTION ( 'NONE',  ( -0.2023178344681547114, 0.9793199139485095905, 8.673617379884032514E-16 ) ) ;
#5218 = CIRCLE ( 'NONE', #3152, 147.0000000000000000 ) ;
#5219 = VECTOR ( 'NONE', #3332, 1000.000000000000000 ) ;
#5220 = VERTEX_POINT ( 'NONE', #4837 ) ;
#5221 = PLANE ( 'NONE',  #2673 ) ;
#5222 = EDGE_CURVE ( 'NONE', #5376, #1906, #1100, .T. ) ;
#5223 = DIRECTION ( 'NONE',  ( 0.9999836672264331705, -0.005715354789860001804, 0.000000000000000000 ) ) ;
#5224 = AXIS2_PLACEMENT_3D ( 'NONE', #6792, #6865, #6383 ) ;
#5225 = DIRECTION ( 'NONE',  ( -5.715354789845005112E-18, -9.999836672264339449E-16, 1.000000000000000000 ) ) ;
#5226 = CARTESIAN_POINT ( 'NONE',  ( -3.268634523084565036, -65.37612200555487618, 3.404282007464019877 ) ) ;
#5227 = LINE ( 'NONE', #5277, #2787 ) ;
#5228 = AXIS2_PLACEMENT_3D ( 'NONE', #5125, #1049, #3301 ) ;
#5229 = CARTESIAN_POINT ( 'NONE',  ( -5.206993624623629913, -63.95781028998001716, 3.417603084305509853 ) ) ;
#5230 = DIRECTION ( 'NONE',  ( 0.8039121061460987594, -0.3550279469270790633, 0.4771587602596087385 ) ) ;
#5231 = ORIENTED_EDGE ( 'NONE', *, *, #3377, .T. ) ;
#5232 = VERTEX_POINT ( 'NONE', #207 ) ;
#5233 = ORIENTED_EDGE ( 'NONE', *, *, #6831, .F. ) ;
#5234 = EDGE_LOOP ( 'NONE', ( #726, #5726 ) ) ;
#5235 = EDGE_CURVE ( 'NONE', #3635, #1686, #1692, .T. ) ;
#5236 = CARTESIAN_POINT ( 'NONE',  ( 18.27210872828645094, -39.59366673520705859, 3.445918334850228693 ) ) ;
#5237 = ORIENTED_EDGE ( 'NONE', *, *, #5138, .T. ) ;
#5238 = CARTESIAN_POINT ( 'NONE',  ( -16.21021049057420882, 1.692961427013491615, 0.006154456448471436192 ) ) ;
#5239 = CARTESIAN_POINT ( 'NONE',  ( -3.365275581743949918, -66.00192919971716776, -0.8990674732841750227 ) ) ;
#5240 = CARTESIAN_POINT ( 'NONE',  ( 27.72433805554270592, -34.20821431467933138, -0.2658584296617393372 ) ) ;
#5241 = CARTESIAN_POINT ( 'NONE',  ( 5.253257825778660184, -59.02147093648149223, -1.455491405082765866 ) ) ;
#5242 = VERTEX_POINT ( 'NONE', #1376 ) ;
#5243 = AXIS2_PLACEMENT_3D ( 'NONE', #6441, #1874, #2369 ) ;
#5244 = ORIENTED_EDGE ( 'NONE', *, *, #5847, .F. ) ;
#5245 = CARTESIAN_POINT ( 'NONE',  ( 27.11783474234811919, -35.12923323413248511, -1.000000000000035083 ) ) ;
#5246 = EDGE_CURVE ( 'NONE', #6942, #7434, #3621, .T. ) ;
#5247 = CARTESIAN_POINT ( 'NONE',  ( -20.89962323070193406, -41.21687045383659154, -3.000000000000042188 ) ) ;
#5248 = CARTESIAN_POINT ( 'NONE',  ( -15.80406914246985650, -35.66025656862317561, -3.000000000000036415 ) ) ;
#5249 = DIRECTION ( 'NONE',  ( 0.05111947575940102573, -0.9986925448795961335, -9.983840675197624659E-16 ) ) ;
#5250 = CARTESIAN_POINT ( 'NONE',  ( 0.000000000000000000, 0.000000000000000000, 3.000000000000000000 ) ) ;
#5251 = CARTESIAN_POINT ( 'NONE',  ( -15.49899450467540163, -35.75040780681265318, -0.4662714048949997969 ) ) ;
#5252 = EDGE_CURVE ( 'NONE', #5988, #6077, #3011, .T. ) ;
#5253 = CARTESIAN_POINT ( 'NONE',  ( -1.005393588828258133, -65.41824993351924888, -2.298700180912566449 ) ) ;
#5254 = CARTESIAN_POINT ( 'NONE',  ( 26.73690888918321207, 2.796431673577179922, 3.035766082959412415E-15 ) ) ;
#5255 = CYLINDRICAL_SURFACE ( 'NONE', #4335, 0.7499999999999994449 ) ;
#5256 = B_SPLINE_SURFACE_WITH_KNOTS ( 'NONE', 3, 3, ( 
 ( #2371, #783, #3569, #5357, #6504, #1876, #189, #4214, #3073, #5884, #5310, #4678, #1350, #6369, #1213, #6962, #705, #4102, #5856, #3494, #2995, #644, #2935, #6405, #4751, #3540, #7258, #7144, #3821, #6112, #6076, #4324, #2551, #3677, #6658, #224, #3105, #7100, #3186, #934, #1456, #7180, #898, #2664, #1505 ),
 ( #4969, #3790, #969, #4934, #5995, #2099, #1421, #1936, #4407, #4252, #3146, #5512, #1980, #6033, #5425, #335, #6695, #6580, #258, #1536, #4859, #6548, #2052, #3711, #4291, #850, #2514, #5470, #300, #4366, #6143, #2015, #5389, #2592, #4899, #6615, #4821, #1390, #3748, #2625, #7218, #3222, #5542, #371, #5577 ),
 ( #525, #2846, #5041, #2706, #6288, #1051, #1128, #2810, #5127, #6219, #3303, #3339, #2126, #7325, #5688, #5651, #2166, #6882, #4557, #7405, #1728, #4477, #414, #4027, #3418, #5164, #5008, #6763, #6252, #6179, #486, #2284, #1615, #1088, #2766, #7290, #4438, #1013, #5079, #4525, #2250, #1573, #7364, #3905, #5620 ),
 ( #5734, #4597, #6841, #1685, #3982, #6328, #2210, #3375, #454, #7440, #3258, #3860, #2734, #6806, #1648, #3942, #562, #1240, #6327, #135, #5301, #2959, #5848, #732, #630, #4774, #7030, #6988, #5272, #3484, #4638, #2429, #1167, #1764, #591, #4133, #1868, #2392, #672, #1831, #3593, #4741, #1896, #4172, #2325 ),
 ( #29, #6434, #1282, #4091, #5907, #2362, #5802, #1202, #5763, #102, #4059, #3451, #6360, #6925, #2920, #3560, #3525, #5875, #2472, #4702, #699, #2988, #5239, #6463, #1308, #3025, #2879, #5344, #7064, #179, #5195, #71, #4671, #6953, #1797, #6396, #6643, #246, #3630, #1412, #3211, #6537, #777, #4202, #3701 ),
 ( #5952, #4957, #1490, #2539, #4809, #5383, #3175, #215, #7091, #807, #6020, #2042, #1444, #885, #2650, #3132, #2615, #1382, #5500, #6604, #359, #324, #4846, #6494, #1342, #6100, #7134, #3670, #838, #4238, #3778, #2006, #2505, #1926, #4888, #3066, #5987, #5452, #1969, #3096, #289, #7169, #5412, #923, #5531 ),
 ( #4315, #6060, #4281, #7243, #6572, #2582, #4924, #7206, #4351, #4997, #5151, #7277, #3248, #5565, #4511, #6751, #5068, #5720, #1038, #6793, #3893, #2116, #3326, #3363, #473, #1525, #5114, #550, #7394, #2195, #6132, #441, #2753, #3811, #400, #4545, #5605, #957, #1605, #1113, #4427, #2693, #2088, #6207, #7312 ),
 ( #1637, #5029, #6167, #2834, #5675, #3927, #4395, #996, #6683, #6715, #2238, #3967, #1559, #2724, #7350, #3848, #2152, #3403, #3289, #513, #4464, #5640, #2796, #6827, #1671, #6277, #4120, #4010, #6947, #5790, #16, #723, #3583, #1270, #6978, #5897, #4051, #2270, #3014, #2979, #1859, #6866, #3476, #2948, #2868 ),
 ( #1193, #5263, #2907, #1711, #6317, #5185, #5226, #1228, #6423, #1158, #1789, #617, #2309, #7428, #62, #5293, #6453, #1821, #3550, #5866, #4581, #4663, #94, #4625, #4162, #1298, #3441, #6915, #6384, #1755, #2354, #127, #4081, #5753, #690, #2418, #3513, #5834, #583, #6351, #662, #4727, #2383, #4693, #7017 ),
 ( #167, #764, #7052, #3123, #870, #1403, #7122, #828, #2606, #1433, #914, #4306, #1333, #798, #6009, #6483, #5440, #276, #3087, #4914, #1371, #2494, #203, #4761, #4273, #3057, #5329, #5371, #3618, #5936, #2573, #2530, #4880, #1476, #6563, #7159, #1959, #4799, #3690, #6594, #1998, #1887, #3166, #3767, #5492 ) ),
 .UNSPECIFIED., .T., .F., .F.,
 ( 4, 2, 2, 2, 4 ),
 ( 4, 3, 2, 2, 2, 2, 2, 2, 2, 2, 2, 2, 2, 2, 2, 2, 2, 2, 2, 2, 2, 4 ),
 ( 0.000000000000000000, 0.2500000000000000000, 0.5000000000000000000, 0.7500000000000000000, 1.000000000000000000 ),
 ( -0.01000000000000000021, 0.000000000000000000, 0.02628634692406570106, 0.07896140836526269191, 0.1315838524972270107, 0.1842089079736879964, 0.2368304666025229932, 0.2894621644501310098, 0.3421084969797454911, 0.3947501728568885149, 0.4473769119526340154, 0.5000000000000000000, 0.5526230880473660401, 0.6052498271431119292, 0.6578915030202550085, 0.7105378355498690457, 0.7631695333974770623, 0.8157910920263119481, 0.8684161475027730726, 0.9210385916347370028, 0.9737136530759340491, 1.000000000000000000 ),
 .UNSPECIFIED. ) ;
#5257 = CARTESIAN_POINT ( 'NONE',  ( -6.321361399357500410, -61.94876894069515316, -0.6341497168666246909 ) ) ;
#5258 = APPLICATION_CONTEXT ( 'automotive_design' ) ;
#5259 = ORIENTED_EDGE ( 'NONE', *, *, #84, .T. ) ;
#5260 = CARTESIAN_POINT ( 'NONE',  ( -5.904042796847299712, -62.42803713013675093, 3.506543003539000392 ) ) ;
#5261 = CARTESIAN_POINT ( 'NONE',  ( -28.70619392989860330, -36.67182071578998404, -3.000000000000037748 ) ) ;
#5262 = CARTESIAN_POINT ( 'NONE',  ( 17.63445134299215056, -39.95697505012468298, -0.2674678461753002279 ) ) ;
#5263 = CARTESIAN_POINT ( 'NONE',  ( -5.595710845088040841, -61.75488600311453524, 3.658668618637090031 ) ) ;
#5264 = CARTESIAN_POINT ( 'NONE',  ( -1.206827191127304078, -66.77204028133226643, -1.044217440639481742 ) ) ;
#5265 = DIRECTION ( 'NONE',  ( 0.9999836672264331705, -0.005715354789860049509, 0.000000000000000000 ) ) ;
#5266 = VERTEX_POINT ( 'NONE', #240 ) ;
#5267 = ADVANCED_FACE ( 'NONE', ( #4801 ), #6050, .T. ) ;
#5268 = EDGE_LOOP ( 'NONE', ( #1565, #6832, #927, #6738, #5878 ) ) ;
#5269 = VERTEX_POINT ( 'NONE', #2033 ) ;
#5270 = FACE_OUTER_BOUND ( 'NONE', #6035, .T. ) ;
#5271 = CYLINDRICAL_SURFACE ( 'NONE', #6646, 5.000000000000000000 ) ;
#5272 = CARTESIAN_POINT ( 'NONE',  ( 6.836834775951150078, -58.56388191083841122, -1.340052733437185895 ) ) ;
#5273 = CARTESIAN_POINT ( 'NONE',  ( 27.21752237596963298, -34.49697494815714549, -0.3076110668159389161 ) ) ;
#5274 = ORIENTED_EDGE ( 'NONE', *, *, #2737, .F. ) ;
#5275 = ORIENTED_EDGE ( 'NONE', *, *, #5690, .T. ) ;
#5276 =( LENGTH_UNIT ( ) NAMED_UNIT ( * ) SI_UNIT ( .MILLI., .METRE. ) );
#5277 = CARTESIAN_POINT ( 'NONE',  ( 30.36903322412724293, 6.222886872815265313, -1.499999999999994227 ) ) ;
#5278 = CYLINDRICAL_SURFACE ( 'NONE', #5243, 11.50000000000000178 ) ;
#5279 = CARTESIAN_POINT ( 'NONE',  ( 41.70778007397900211, -94.98992620957551480, 2.999999999999905409 ) ) ;
#5280 = DIRECTION ( 'NONE',  ( 0.000000000000000000, 0.000000000000000000, -1.000000000000000000 ) ) ;
#5281 = CARTESIAN_POINT ( 'NONE',  ( -9.311346830843410416, -51.41373841511902043, 2.533728595105000370 ) ) ;
#5282 = ORIENTED_EDGE ( 'NONE', *, *, #738, .T. ) ;
#5283 = EDGE_CURVE ( 'NONE', #5220, #7266, #7085, .T. ) ;
#5284 = SHAPE_REPRESENTATION ( 'Vinyl Handle Grips', ( #751 ), #989 ) ;
#5285 = CARTESIAN_POINT ( 'NONE',  ( 1.159677199572074269, -55.50330010691895666, -1.238196965061255650 ) ) ;
#5286 = CARTESIAN_POINT ( 'NONE',  ( 14.63763862841555330, 20.11382921380837985, -2.993845543551509447 ) ) ;
#5287 = CARTESIAN_POINT ( 'NONE',  ( 5.463696144088109996, -62.30361170774578028, -3.475027489484119769 ) ) ;
#5288 = CARTESIAN_POINT ( 'NONE',  ( 94.42889356597736139, -103.2882618349535591, -3.000000000000103917 ) ) ;
#5289 = CARTESIAN_POINT ( 'NONE',  ( 15.26844188666829893, -16.88471001685938688, 2.999999999999983125 ) ) ;
#5290 = ADVANCED_FACE ( 'NONE', ( #3060 ), #5980, .F. ) ;
#5291 = EDGE_LOOP ( 'NONE', ( #487, #3685, #3853, #449 ) ) ;
#5292 = DIRECTION ( 'NONE',  ( -0.4039838799357092780, -0.9147661038495525920, 4.517316048719004797E-16 ) ) ;
#5293 = CARTESIAN_POINT ( 'NONE',  ( 1.626596344682255113, -54.75750786503496670, 2.255510009909589719 ) ) ;
#5294 = CARTESIAN_POINT ( 'NONE',  ( -5.354034084503060065, -64.02545556441495478, -0.7792797212839647214 ) ) ;
#5295 = DIRECTION ( 'NONE',  ( 5.715354789860003484E-18, 9.999836672264337477E-16, -1.000000000000000000 ) ) ;
#5296 = ORIENTED_EDGE ( 'NONE', *, *, #3089, .F. ) ;
#5297 = ORIENTED_EDGE ( 'NONE', *, *, #3679, .T. ) ;
#5298 = VECTOR ( 'NONE', #7376, 1000.000000000000000 ) ;
#5299 = DIRECTION ( 'NONE',  ( 0.3128463504745289114, 0.9445772445362836667, 0.09950371902099885979 ) ) ;
#5300 = CARTESIAN_POINT ( 'NONE',  ( -10.54744521951312208, -8.271218886098244738, -3.000000000000009326 ) ) ;
#5301 = CARTESIAN_POINT ( 'NONE',  ( -6.891320273265630014, -62.11321098440852495, -0.2797727661029551505 ) ) ;
#5302 = DIRECTION ( 'NONE',  ( -0.2344748185227520099, 0.9721221936972339606, 0.000000000000000000 ) ) ;
#5303 = AXIS2_PLACEMENT_3D ( 'NONE', #4688, #7419, #2859 ) ;
#5304 = EDGE_LOOP ( 'NONE', ( #7092, #6807 ) ) ;
#5305 = ORIENTED_EDGE ( 'NONE', *, *, #837, .T. ) ;
#5306 = DIRECTION ( 'NONE',  ( -5.715354789845005112E-18, -9.999836672264339449E-16, 1.000000000000000000 ) ) ;
#5307 = ADVANCED_FACE ( 'NONE', ( #4308 ), #3169, .T. ) ;
#5308 = DIRECTION ( 'NONE',  ( -0.7411265327553895332, -0.6713653717953993461, -1.302304562955136699E-15 ) ) ;
#5309 = CARTESIAN_POINT ( 'NONE',  ( 5.930474762900869834, -62.46354786334135412, -3.475732462342234985 ) ) ;
#5310 = CARTESIAN_POINT ( 'NONE',  ( 5.416018991692120643, -63.93240027730202968, 2.754852738177090643 ) ) ;
#5311 = EDGE_LOOP ( 'NONE', ( #5535, #4018, #4567, #7237, #906, #5796 ) ) ;
#5312 = ADVANCED_BREP_SHAPE_REPRESENTATION ( '', ( #2417, #751 ), #1245 ) ;
#5313 = CARTESIAN_POINT ( 'NONE',  ( 2.751515497641074948, -64.99867735210931130, 0.5749532485596650089 ) ) ;
#5314 = ADVANCED_FACE ( 'NONE', ( #6596 ), #830, .T. ) ;
#5315 = DIRECTION ( 'NONE',  ( 0.7411265327553895332, 0.6713653717953992350, 6.755902076156661002E-16 ) ) ;
#5316 = EDGE_CURVE ( 'NONE', #3385, #70, #1577, .T. ) ;
#5317 = DIRECTION ( 'NONE',  ( 5.715354789845005112E-18, 9.999836672264339449E-16, -1.000000000000000000 ) ) ;
#5318 = CARTESIAN_POINT ( 'NONE',  ( -4.705238872764143210, -56.98302411029121828, -0.2229714063405454361 ) ) ;
#5319 = CARTESIAN_POINT ( 'NONE',  ( -5.727966693761760375, -63.15494832584334262, 1.398024598501910187 ) ) ;
#5320 = DIRECTION ( 'NONE',  ( -0.9999836672264332815, 0.005715354789860036498, 0.000000000000000000 ) ) ;
#5321 = ORIENTED_EDGE ( 'NONE', *, *, #4532, .F. ) ;
#5322 = CIRCLE ( 'NONE', #7113, 147.0000000000000000 ) ;
#5323 = DIRECTION ( 'NONE',  ( -0.3144019573014841806, 0.9492899500389728740, 0.000000000000000000 ) ) ;
#5324 = EDGE_CURVE ( 'NONE', #2342, #5842, #5803, .T. ) ;
#5325 = CARTESIAN_POINT ( 'NONE',  ( 27.74658554044268399, 26.69867264686258679, -2.152344182241802795 ) ) ;
#5326 = CARTESIAN_POINT ( 'NONE',  ( 17.85753840846644636, -40.40533092278068494, -0.5000000000000403011 ) ) ;
#5327 = UNCERTAINTY_MEASURE_WITH_UNIT (LENGTH_MEASURE( 1.000000000000000082E-05 ), #3858, 'distance_accuracy_value', 'NONE');
#5328 = CIRCLE ( 'NONE', #6418, 4.000000000000000000 ) ;
#5329 = CARTESIAN_POINT ( 'NONE',  ( 5.619938529503549773, -63.59344562873818774, 0.6343307546824898946 ) ) ;
#5330 = CIRCLE ( 'NONE', #6299, 6.300000000000001599 ) ;
#5331 = CARTESIAN_POINT ( 'NONE',  ( 3.331090576803830139, -65.95739139720836874, 0.8111086825117052035 ) ) ;
#5332 = PLANE ( 'NONE',  #6984 ) ;
#5333 = ORIENTED_EDGE ( 'NONE', *, *, #4680, .T. ) ;
#5334 = CIRCLE ( 'NONE', #2067, 2.249999999999996891 ) ;
#5335 = ORIENTED_EDGE ( 'NONE', *, *, #6919, .F. ) ;
#5336 = ORIENTED_EDGE ( 'NONE', *, *, #6230, .T. ) ;
#5337 = ORIENTED_EDGE ( 'NONE', *, *, #3705, .F. ) ;
#5338 = VECTOR ( 'NONE', #1192, 1000.000000000000000 ) ;
#5339 = AXIS2_PLACEMENT_3D ( 'NONE', #6139, #3856, #6072 ) ;
#5340 = LINE ( 'NONE', #7089, #994 ) ;
#5341 = VERTEX_POINT ( 'NONE', #2077 ) ;
#5342 = CONICAL_SURFACE ( 'NONE', #759, 0.7499999999999863443, 1.029744258676653645 ) ;
#5343 = DIRECTION ( 'NONE',  ( -5.715354789860003484E-18, -9.999836672264337477E-16, 1.000000000000000000 ) ) ;
#5344 = CARTESIAN_POINT ( 'NONE',  ( 6.291895255447879975, -62.07086823355334104, -1.517278733858541839 ) ) ;
#5345 = CARTESIAN_POINT ( 'NONE',  ( 20.29543457672885154, -41.45429371584161515, -3.001370543551582060 ) ) ;
#5346 = ORIENTED_EDGE ( 'NONE', *, *, #4602, .T. ) ;
#5347 = VECTOR ( 'NONE', #2639, 1000.000000000000227 ) ;
#5348 = CONICAL_SURFACE ( 'NONE', #4744, 0.7500000000000002220, 1.029744258676651425 ) ;
#5349 = VERTEX_POINT ( 'NONE', #6094 ) ;
#5350 = VERTEX_POINT ( 'NONE', #2643 ) ;
#5351 = VECTOR ( 'NONE', #260, 1000.000000000000227 ) ;
#5352 = SHAPE_REPRESENTATION_RELATIONSHIP ( 'NONE' , 'NONE' ,  #4460, #4410 ) ;
#5353 = DIRECTION ( 'NONE',  ( -0.3144019573014843472, 0.9492899500389728740, 0.000000000000000000 ) ) ;
#5354 = DIRECTION ( 'NONE',  ( -0.4039838799357104993, -0.9147661038495521479, -1.912040383129595888E-16 ) ) ;
#5355 = AXIS2_PLACEMENT_3D ( 'NONE', #1515, #4945, #3423 ) ;
#5356 = CARTESIAN_POINT ( 'NONE',  ( 10.07902270299396008, 17.77910117033601978, 2.236547809770398132 ) ) ;
#5357 = CARTESIAN_POINT ( 'NONE',  ( -5.895051854024569771, -62.45358532148892294, 3.505907163650189950 ) ) ;
#5358 = CARTESIAN_POINT ( 'NONE',  ( 0.000000000000000000, 0.000000000000000000, 3.000000000000000000 ) ) ;
#5359 = EDGE_CURVE ( 'NONE', #7317, #4841, #4389, .T. ) ;
#5360 = CARTESIAN_POINT ( 'NONE',  ( -2.961840227416660198, -65.56364223063081909, 1.283932781279834900 ) ) ;
#5361 = CARTESIAN_POINT ( 'NONE',  ( 13.75494557961500419, 19.53026195111434404, -2.993845543551520105 ) ) ;
#5362 = CARTESIAN_POINT ( 'NONE',  ( 4.814269575835951720, -62.05762139399459443, -2.948265134628040407 ) ) ;
#5363 = CARTESIAN_POINT ( 'NONE',  ( -4.722210582817570668, -63.78749880788215876, -2.740498917967187698 ) ) ;
#5364 = CARTESIAN_POINT ( 'NONE',  ( 1.600318488538475137, -66.74162401608067796, -1.164216807110747931 ) ) ;
#5365 = ORIENTED_EDGE ( 'NONE', *, *, #5502, .T. ) ;
#5366 = ADVANCED_FACE ( 'NONE', ( #2183 ), #1520, .T. ) ;
#5367 = CARTESIAN_POINT ( 'NONE',  ( 15.01043771185145381, 6.851040774847843906, 6.938893903907228378E-15 ) ) ;
#5368 = CARTESIAN_POINT ( 'NONE',  ( 27.30483170388682979, -34.44723004512030684, 2.999999999999965805 ) ) ;
#5369 = CARTESIAN_POINT ( 'NONE',  ( -4.860610968486169803, -1.172374092613760022, -17.67054229618195293 ) ) ;
#5370 = DIRECTION ( 'NONE',  ( -0.9721221936972339606, -0.2344748185227520099, 0.000000000000000000 ) ) ;
#5371 = CARTESIAN_POINT ( 'NONE',  ( 6.265638173095489982, -61.94185186372677521, 0.5461908750427398873 ) ) ;
#5372 = CARTESIAN_POINT ( 'NONE',  ( -4.747117373927349782, -63.10583374278928659, -0.4844647803776696016 ) ) ;
#5373 = CARTESIAN_POINT ( 'NONE',  ( -5.895051854024569771, -62.45358532148892294, 3.505907163650189950 ) ) ;
#5374 = LINE ( 'NONE', #4228, #1449 ) ;
#5375 = EDGE_LOOP ( 'NONE', ( #2506, #1391, #5244, #4467 ) ) ;
#5376 = VERTEX_POINT ( 'NONE', #2745 ) ;
#5377 = EDGE_CURVE ( 'NONE', #184, #2611, #5711, .T. ) ;
#5378 = EDGE_CURVE ( 'NONE', #3100, #6173, #2414, .T. ) ;
#5379 = VERTEX_POINT ( 'NONE', #2230 ) ;
#5380 = ORIENTED_EDGE ( 'NONE', *, *, #2398, .F. ) ;
#5381 = CARTESIAN_POINT ( 'NONE',  ( -95.86211798318534250, -102.0316339954322018, -1.027823659516258203E-13 ) ) ;
#5382 = LINE ( 'NONE', #1968, #6180 ) ;
#5383 = CARTESIAN_POINT ( 'NONE',  ( -4.450126406946254498, -63.33667035482537244, 1.592103300391294773 ) ) ;
#5384 = ORIENTED_EDGE ( 'NONE', *, *, #836, .T. ) ;
#5385 = ORIENTED_EDGE ( 'NONE', *, *, #4805, .F. ) ;
#5386 = DIRECTION ( 'NONE',  ( -0.9999836672264335036, 0.005715354789845041548, 0.000000000000000000 ) ) ;
#5387 = DIRECTION ( 'NONE',  ( -0.9721221936972339606, -0.2344748185227520099, 0.000000000000000000 ) ) ;
#5388 = CARTESIAN_POINT ( 'NONE',  ( 5.001731546698911401, -62.07693240093809806, -1.811760589978133051 ) ) ;
#5389 = CARTESIAN_POINT ( 'NONE',  ( -2.038541806680159940, -53.77797276486428046, -0.2805255711276150588 ) ) ;
#5390 = FACE_OUTER_BOUND ( 'NONE', #2203, .T. ) ;
#5391 = CARTESIAN_POINT ( 'NONE',  ( -1.397697773942189858, -54.69607029038206747, 2.078897745975250455 ) ) ;
#5392 = SURFACE_SIDE_STYLE ('',( #6176 ) ) ;
#5393 = DIRECTION ( 'NONE',  ( -0.6713653717953970146, 0.7411265327553913096, 7.633377738797892154E-16 ) ) ;
#5394 = CARTESIAN_POINT ( 'NONE',  ( -5.758700247327861454, -59.47069914579707017, -2.478271157609042596 ) ) ;
#5395 = ORIENTED_EDGE ( 'NONE', *, *, #4302, .T. ) ;
#5396 = DIRECTION ( 'NONE',  ( -0.9147661038495522590, 0.4039838799357101107, 0.000000000000000000 ) ) ;
#5397 = DIRECTION ( 'NONE',  ( -5.715354789860003484E-18, -9.999836672264337477E-16, 1.000000000000000000 ) ) ;
#5398 = CARTESIAN_POINT ( 'NONE',  ( 18.63383769599579054, -39.96626706310059518, -1.000000000000039746 ) ) ;
#5399 = EDGE_CURVE ( 'NONE', #1922, #2186, #3611, .T. ) ;
#5400 = UNCERTAINTY_MEASURE_WITH_UNIT (LENGTH_MEASURE( 1.000000000000000082E-05 ), #4209, 'distance_accuracy_value', 'NONE');
#5401 = CYLINDRICAL_SURFACE ( 'NONE', #122, 6.299999999999997158 ) ;
#5402 = CARTESIAN_POINT ( 'NONE',  ( 3.949972843796054178, -66.18831294452250802, -1.427832076542613793 ) ) ;
#5403 = CARTESIAN_POINT ( 'NONE',  ( 13.32147353159843028, 12.06754263290683937, -0.3999035282155026794 ) ) ;
#5404 = EDGE_LOOP ( 'NONE', ( #46, #7102, #3178, #3757 ) ) ;
#5405 = VERTEX_POINT ( 'NONE', #545 ) ;
#5406 = ORIENTED_EDGE ( 'NONE', *, *, #5689, .T. ) ;
#5407 = CYLINDRICAL_SURFACE ( 'NONE', #48, 4.000000000000000000 ) ;
#5408 = AXIS2_PLACEMENT_3D ( 'NONE', #2220, #49, #5740 ) ;
#5409 = LINE ( 'NONE', #6536, #4243 ) ;
#5410 = EDGE_CURVE ( 'NONE', #75, #4478, #1026, .T. ) ;
#5411 = ADVANCED_FACE ( 'NONE', ( #6677 ), #6199, .T. ) ;
#5412 = CARTESIAN_POINT ( 'NONE',  ( 4.396896920912054973, -63.41639021975223045, -3.266830536337445245 ) ) ;
#5413 = CARTESIAN_POINT ( 'NONE',  ( 3.692193437564742275, -55.33181466697134709, 0.1491418217178651084 ) ) ;
#5414 = ORIENTED_EDGE ( 'NONE', *, *, #5477, .T. ) ;
#5415 = ORIENTED_EDGE ( 'NONE', *, *, #5131, .T. ) ;
#5416 = ORIENTED_EDGE ( 'NONE', *, *, #3735, .F. ) ;
#5417 = ORIENTED_EDGE ( 'NONE', *, *, #303, .T. ) ;
#5418 = VECTOR ( 'NONE', #3277, 1000.000000000000000 ) ;
#5419 = SHAPE_REPRESENTATION_RELATIONSHIP ( 'NONE' , 'NONE' ,  #2136, #5312 ) ;
#5420 = CARTESIAN_POINT ( 'NONE',  ( -9.232392015783828398, 12.99354368604250887, 5.337608095967012467 ) ) ;
#5421 = EDGE_CURVE ( 'NONE', #6025, #5269, #2567, .T. ) ;
#5422 = FACE_OUTER_BOUND ( 'NONE', #3906, .T. ) ;
#5423 = CIRCLE ( 'NONE', #4819, 3.750000000000000444 ) ;
#5424 = DIRECTION ( 'NONE',  ( -0.9147661038495489283, 0.4039838799357176602, 3.987490689252441100E-16 ) ) ;
#5425 = CARTESIAN_POINT ( 'NONE',  ( 3.691078954254495059, -54.53160935192415337, 2.105200478230089267 ) ) ;
#5426 = ORIENTED_EDGE ( 'NONE', *, *, #5006, .T. ) ;
#5427 = AXIS2_PLACEMENT_3D ( 'NONE', #3516, #5755, #5792 ) ;
#5428 = CARTESIAN_POINT ( 'NONE',  ( 7.283874945971848369, -8.906884184084093548, -3.000000000000009770 ) ) ;
#5429 = CARTESIAN_POINT ( 'NONE',  ( -4.559578989909869762, -57.69789612496867903, 1.459412177499654462 ) ) ;
#5430 = EDGE_CURVE ( 'NONE', #1273, #7056, #2926, .T. ) ;
#5431 = FACE_OUTER_BOUND ( 'NONE', #2003, .T. ) ;
#5432 = CARTESIAN_POINT ( 'NONE',  ( -5.212048506017270100, -63.07061735744050424, -0.5901561396984810193 ) ) ;
#5433 = PRODUCT_DEFINITION_SHAPE ( 'NONE', 'NONE',  #5465 ) ;
#5434 = VERTEX_POINT ( 'NONE', #6233 ) ;
#5435 = CARTESIAN_POINT ( 'NONE',  ( -28.02385480137100160, 13.25058454003099939, -1.493845543551999944 ) ) ;
#5436 = AXIS2_PLACEMENT_3D ( 'NONE', #5716, #3437, #6348 ) ;
#5437 = DIRECTION ( 'NONE',  ( 0.000000000000000000, 0.000000000000000000, -1.000000000000000000 ) ) ;
#5438 = DIRECTION ( 'NONE',  ( -0.7411265327553894222, -0.6713653717953992350, -1.302304562955136501E-15 ) ) ;
#5439 = CARTESIAN_POINT ( 'NONE',  ( -30.62055434958606170, 13.52281233407238403, -8.815182418718723767 ) ) ;
#5440 = CARTESIAN_POINT ( 'NONE',  ( -1.512046953658800152, -54.18079592905042574, 1.959428465566195543 ) ) ;
#5441 = CARTESIAN_POINT ( 'NONE',  ( -3.403807323753265113, -54.36107883567960641, 1.752763223655470437 ) ) ;
#5442 = CARTESIAN_POINT ( 'NONE',  ( 18.04796579205319063, 16.34913706177017190, 3.306154456448485490 ) ) ;
#5443 = VECTOR ( 'NONE', #6130, 1000.000000000000227 ) ;
#5444 = CIRCLE ( 'NONE', #2670, 0.5000000000000022204 ) ;
#5445 = ORIENTED_EDGE ( 'NONE', *, *, #5460, .T. ) ;
#5446 = ORIENTED_EDGE ( 'NONE', *, *, #3053, .F. ) ;
#5447 = EDGE_CURVE ( 'NONE', #2713, #2395, #2143, .T. ) ;
#5448 = LINE ( 'NONE', #4313, #2301 ) ;
#5449 = AXIS2_PLACEMENT_3D ( 'NONE', #3954, #6264, #1102 ) ;
#5450 = VECTOR ( 'NONE', #1375, 1000.000000000000000 ) ;
#5451 = DIRECTION ( 'NONE',  ( 5.715354789845005112E-18, 9.999836672264339449E-16, -1.000000000000000000 ) ) ;
#5452 = CARTESIAN_POINT ( 'NONE',  ( -4.574768583212910578, -63.39215034952142247, -2.605000795493774834 ) ) ;
#5453 = CARTESIAN_POINT ( 'NONE',  ( 3.293998498883576875, -65.74688398529977462, 0.8048007446836616952 ) ) ;
#5454 = ORIENTED_EDGE ( 'NONE', *, *, #4495, .T. ) ;
#5455 = CIRCLE ( 'NONE', #3754, 3.250000000000000888 ) ;
#5456 = ORIENTED_EDGE ( 'NONE', *, *, #676, .F. ) ;
#5457 = ORIENTED_EDGE ( 'NONE', *, *, #5607, .T. ) ;
#5458 = CIRCLE ( 'NONE', #5339, 3.750000000000000000 ) ;
#5459 = EDGE_CURVE ( 'NONE', #6398, #5505, #765, .T. ) ;
#5460 = EDGE_CURVE ( 'NONE', #4310, #1236, #4379, .T. ) ;
#5461 = PRODUCT_DEFINITION_FORMATION_WITH_SPECIFIED_SOURCE ( 'ANY', '', #729, .NOT_KNOWN. ) ;
#5462 = AXIS2_PLACEMENT_3D ( 'NONE', #7404, #3979, #5575 ) ;
#5463 = DIRECTION ( 'NONE',  ( 1.000000000000000000, 0.000000000000000000, 0.000000000000000000 ) ) ;
#5464 = DIRECTION ( 'NONE',  ( 0.9999836672264333925, -0.005715354789844381486, 0.000000000000000000 ) ) ;
#5465 = PRODUCT_DEFINITION ( 'UNKNOWN', '', #2441, #3201 ) ;
#5466 = CIRCLE ( 'NONE', #2329, 1.000000000000000000 ) ;
#5467 = PLANE ( 'NONE',  #5851 ) ;
#5468 = VECTOR ( 'NONE', #1600, 1000.000000000000000 ) ;
#5469 = CARTESIAN_POINT ( 'NONE',  ( 4.748085323256989732, -62.01668842780453872, -2.502390571778199568 ) ) ;
#5470 = CARTESIAN_POINT ( 'NONE',  ( 6.775879105374429834, -62.07729961717699041, 0.4273099905340951299 ) ) ;
#5471 = EDGE_LOOP ( 'NONE', ( #4358, #3208, #5034, #3223 ) ) ;
#5472 = AXIS2_PLACEMENT_3D ( 'NONE', #466, #3842, #4990 ) ;
#5473 = VECTOR ( 'NONE', #5811, 1000.000000000000000 ) ;
#5474 = ORIENTED_EDGE ( 'NONE', *, *, #2873, .T. ) ;
#5475 = ORIENTED_EDGE ( 'NONE', *, *, #2605, .F. ) ;
#5476 = ADVANCED_FACE ( 'NONE', ( #4422 ), #5668, .T. ) ;
#5477 = EDGE_CURVE ( 'NONE', #4883, #3069, #2265, .T. ) ;
#5478 = DIRECTION ( 'NONE',  ( 0.8133302887613500509, 0.5818022356294096920, 5.864412043468331297E-16 ) ) ;
#5479 = CARTESIAN_POINT ( 'NONE',  ( -5.250750166908019878, -57.72135505925717069, -0.3064819419056146188 ) ) ;
#5480 = VECTOR ( 'NONE', #5696, 1000.000000000000000 ) ;
#5481 = ORIENTED_EDGE ( 'NONE', *, *, #2167, .T. ) ;
#5482 = DIRECTION ( 'NONE',  ( 1.000000000000000000, 0.000000000000000000, 0.000000000000000000 ) ) ;
#5483 = CARTESIAN_POINT ( 'NONE',  ( 14.49911764349215915, -35.75048010860329839, 2.597518595105000383 ) ) ;
#5484 = CARTESIAN_POINT ( 'NONE',  ( 5.463205525817310892, -58.24907413091714403, -1.612795058816904437 ) ) ;
#5485 = AXIS2_PLACEMENT_3D ( 'NONE', #2050, #6578, #5387 ) ;
#5486 = VERTEX_POINT ( 'NONE', #5600 ) ;
#5487 = EDGE_CURVE ( 'NONE', #3871, #1452, #6785, .T. ) ;
#5488 = DIRECTION ( 'NONE',  ( 0.7411265327553895332, 0.6713653717953993461, 1.302304562955136699E-15 ) ) ;
#5489 = DIRECTION ( 'NONE',  ( 0.000000000000000000, 0.000000000000000000, -1.000000000000000000 ) ) ;
#5490 = CARTESIAN_POINT ( 'NONE',  ( -14.07431766324681988, -37.03265636863024923, 1.026284428608169819 ) ) ;
#5491 = PRODUCT_DEFINITION_CONTEXT ( 'detailed design', #1111, 'design' ) ;
#5492 = CARTESIAN_POINT ( 'NONE',  ( 5.929218414971320072, -62.35084102844776055, -1.530333388185332932 ) ) ;
#5493 = CARTESIAN_POINT ( 'NONE',  ( 27.12559638130199247, -35.12481100358304076, -1.000000000000035083 ) ) ;
#5494 = CARTESIAN_POINT ( 'NONE',  ( 3.357456528971034970, -66.96770758659590683, 2.241359037429140333 ) ) ;
#5495 = DIRECTION ( 'NONE',  ( -1.850371707708594129E-14, -4.625929269271485795E-14, 1.000000000000000000 ) ) ;
#5496 = VERTEX_POINT ( 'NONE', #1629 ) ;
#5497 = EDGE_LOOP ( 'NONE', ( #1816, #2252, #4267, #33 ) ) ;
#5498 = CARTESIAN_POINT ( 'NONE',  ( -12.11759654540111875, 13.15705282150456590, 3.000000000000013767 ) ) ;
#5499 = DIRECTION ( 'NONE',  ( -5.715354789845005112E-18, -9.999836672264339449E-16, 1.000000000000000000 ) ) ;
#5500 = CARTESIAN_POINT ( 'NONE',  ( -4.614416121558960526, -57.55752852796073427, -0.1302737383155048445 ) ) ;
#5501 = DIRECTION ( 'NONE',  ( -0.4039838799357194921, -0.9147661038495481511, 5.438507216189340937E-17 ) ) ;
#5502 = EDGE_CURVE ( 'NONE', #7163, #7292, #3921, .T. ) ;
#5503 = CARTESIAN_POINT ( 'NONE',  ( -0.06384554175070766835, -54.19636094766362078, 2.037209790278620591 ) ) ;
#5504 = EDGE_LOOP ( 'NONE', ( #4766, #3672, #199, #2055 ) ) ;
#5505 = VERTEX_POINT ( 'NONE', #5104 ) ;
#5506 = VERTEX_POINT ( 'NONE', #7387 ) ;
#5507 =( LENGTH_UNIT ( ) NAMED_UNIT ( * ) SI_UNIT ( .MILLI., .METRE. ) );
#5508 = DIRECTION ( 'NONE',  ( 0.4039838799357109433, 0.9147661038495520369, 9.170600743851225078E-16 ) ) ;
#5509 = DIRECTION ( 'NONE',  ( 1.153459499832656523E-16, -1.000675586835500184E-15, 1.000000000000000000 ) ) ;
#5510 = B_SPLINE_CURVE_WITH_KNOTS ( 'NONE', 3,
 ( #3832, #3349, #5589, #1467, #5627, #459, #426, #2712, #5092, #944, #3760, #5050 ),
 .UNSPECIFIED., .F., .F.,
 ( 4, 2, 2, 2, 2, 4 ),
 ( 0.000000000000000000, 0.1249999999999981404, 0.2499999999999962808, 0.4999999999999954481, 0.7499999999999976685, 1.000000000000000000 ),
 .UNSPECIFIED. ) ;
#5511 = CARTESIAN_POINT ( 'NONE',  ( 10.02759472486470926, 5.630039434485816230, 5.687258741868093102E-15 ) ) ;
#5512 = CARTESIAN_POINT ( 'NONE',  ( 6.663059173928499668, -62.48704134639812935, 2.547684199221960100 ) ) ;
#5513 = EDGE_LOOP ( 'NONE', ( #1921, #4885 ) ) ;
#5514 = DIRECTION ( 'NONE',  ( -5.715354789845005112E-18, -9.999836672264339449E-16, 1.000000000000000000 ) ) ;
#5515 = CARTESIAN_POINT ( 'NONE',  ( 5.661113010068490325, -57.37064013373739613, 2.401523511004880262 ) ) ;
#5516 = DIRECTION ( 'NONE',  ( 0.9999836672264331705, -0.005715354789860049509, 0.000000000000000000 ) ) ;
#5517 = ADVANCED_FACE ( 'NONE', ( #1663 ), #6269, .T. ) ;
#5518 = EDGE_CURVE ( 'NONE', #3357, #1468, #1487, .T. ) ;
#5519 = CARTESIAN_POINT ( 'NONE',  ( 104.0973215944787711, -119.5240462704291389, -1.189271409856590718E-13 ) ) ;
#5520 = VERTEX_POINT ( 'NONE', #4657 ) ;
#5521 = DIRECTION ( 'NONE',  ( -0.9147661038495482622, 0.4039838799357193255, 3.987490689252457863E-16 ) ) ;
#5522 = FACE_OUTER_BOUND ( 'NONE', #4309, .T. ) ;
#5523 = DIRECTION ( 'NONE',  ( -5.715354789860003484E-18, -9.999836672264337477E-16, 1.000000000000000000 ) ) ;
#5524 = FACE_BOUND ( 'NONE', #4348, .T. ) ;
#5525 = CARTESIAN_POINT ( 'NONE',  ( 6.802585521241110378, -58.92636561181245014, 2.370308086683080351 ) ) ;
#5526 = CARTESIAN_POINT ( 'NONE',  ( 14.38741851828413942, 8.077882666870964457, -2.999999999999992895 ) ) ;
#5527 = ORIENTED_EDGE ( 'NONE', *, *, #5886, .T. ) ;
#5528 = ORIENTED_EDGE ( 'NONE', *, *, #5702, .T. ) ;
#5529 = DIRECTION ( 'NONE',  ( -0.5224671166576538850, 0.8526594349512809368, 0.000000000000000000 ) ) ;
#5530 = CARTESIAN_POINT ( 'NONE',  ( -1.172374092613760022, 4.860610968486169803, -3.000000000000000000 ) ) ;
#5531 = CARTESIAN_POINT ( 'NONE',  ( 4.980378365057210210, -62.14367890036703557, -3.355420260138584521 ) ) ;
#5532 = DIRECTION ( 'NONE',  ( 0.9999836672264332815, -0.005715354789847320975, 0.000000000000000000 ) ) ;
#5533 = CARTESIAN_POINT ( 'NONE',  ( -5.001340985743557788, -64.18787007827532420, 3.400789707794877881 ) ) ;
#5534 = CARTESIAN_POINT ( 'NONE',  ( -1.334494426138621792, -66.80443255658586565, -3.107681693547102775 ) ) ;
#5535 = ORIENTED_EDGE ( 'NONE', *, *, #217, .F. ) ;
#5536 = ORIENTED_EDGE ( 'NONE', *, *, #1458, .T. ) ;
#5537 = ORIENTED_EDGE ( 'NONE', *, *, #5730, .F. ) ;
#5538 = CIRCLE ( 'NONE', #2516, 17.99999999999999645 ) ;
#5539 = CARTESIAN_POINT ( 'NONE',  ( 15.94457129749017277, -41.07922723232461237, -4.119968255444916849E-14 ) ) ;
#5540 = DIRECTION ( 'NONE',  ( 0.9999836672264332815, -0.005715354789845002517, 0.000000000000000000 ) ) ;
#5541 = DIRECTION ( 'NONE',  ( 5.715354789860003484E-18, 9.999836672264337477E-16, -1.000000000000000000 ) ) ;
#5542 = CARTESIAN_POINT ( 'NONE',  ( 5.693513582185560473, -64.15546253253084785, -1.561391656022143914 ) ) ;
#5543 = AXIS2_PLACEMENT_3D ( 'NONE', #4226, #6524, #2029 ) ;
#5544 = VERTEX_POINT ( 'NONE', #55 ) ;
#5545 = EDGE_CURVE ( 'NONE', #418, #6505, #882, .T. ) ;
#5546 = DIRECTION ( 'NONE',  ( -0.1248576012279780517, 0.9921746718272922427, 1.096417580487671857E-15 ) ) ;
#5547 = CARTESIAN_POINT ( 'NONE',  ( 1.700848490796859958, -66.65813550864595527, 0.8993149516912349872 ) ) ;
#5548 = VECTOR ( 'NONE', #3267, 1000.000000000000000 ) ;
#5549 = CARTESIAN_POINT ( 'NONE',  ( -32.93157973858376408, 14.54341967768581867, -2.999999999999986677 ) ) ;
#5550 = CARTESIAN_POINT ( 'NONE',  ( -3.888488774788935842, -0.9378992740910081505, -3.000000000000000000 ) ) ;
#5551 = AXIS2_PLACEMENT_3D ( 'NONE', #692, #129, #1890 ) ;
#5552 = ORIENTED_EDGE ( 'NONE', *, *, #2131, .F. ) ;
#5553 = ADVANCED_FACE ( 'NONE', ( #2299 ), #1186, .T. ) ;
#5554 = EDGE_CURVE ( 'NONE', #5544, #6347, #5835, .T. ) ;
#5555 = CARTESIAN_POINT ( 'NONE',  ( 13.19545720709724890, -35.82600185752891520, -3.556183125752454544E-14 ) ) ;
#5556 = LINE ( 'NONE', #6266, #4699 ) ;
#5557 = CARTESIAN_POINT ( 'NONE',  ( 20.29543457672885154, -41.45429371584162226, -4.119968255444916849E-14 ) ) ;
#5558 = CARTESIAN_POINT ( 'NONE',  ( -6.268616217933410617, -56.62827303305337523, 1.003072567477500066 ) ) ;
#5559 = DIRECTION ( 'NONE',  ( 0.9999836672264333925, -0.005715354789860572528, 0.000000000000000000 ) ) ;
#5560 = VERTEX_POINT ( 'NONE', #5289 ) ;
#5561 = EDGE_LOOP ( 'NONE', ( #1777, #3519 ) ) ;
#5562 = EDGE_CURVE ( 'NONE', #6173, #4319, #3532, .T. ) ;
#5563 = LINE ( 'NONE', #4462, #264 ) ;
#5564 = CARTESIAN_POINT ( 'NONE',  ( 27.65533861039806496, -36.12687000486608468, -3.599551212651874721E-14 ) ) ;
#5565 = CARTESIAN_POINT ( 'NONE',  ( 4.485945982887084682, -58.07227379738043993, 1.147183751133595386 ) ) ;
#5566 = CARTESIAN_POINT ( 'NONE',  ( 27.30483166554891739, -34.44723006696351320, 3.065403626746449728 ) ) ;
#5567 = CARTESIAN_POINT ( 'NONE',  ( 0.000000000000000000, 0.000000000000000000, -2.544444444444450060 ) ) ;
#5568 = ORIENTED_EDGE ( 'NONE', *, *, #3932, .T. ) ;
#5569 = ORIENTED_EDGE ( 'NONE', *, *, #827, .T. ) ;
#5570 = ORIENTED_EDGE ( 'NONE', *, *, #1939, .T. ) ;
#5571 = VECTOR ( 'NONE', #2295, 1000.000000000000000 ) ;
#5572 = CONICAL_SURFACE ( 'NONE', #2908, 0.7499999999999863443, 1.029744258676653645 ) ;
#5573 = FACE_OUTER_BOUND ( 'NONE', #6439, .T. ) ;
#5574 = VECTOR ( 'NONE', #4342, 1000.000000000000114 ) ;
#5575 = DIRECTION ( 'NONE',  ( -5.313805496780495629E-16, -9.969792550665913157E-16, 1.000000000000000000 ) ) ;
#5576 = CARTESIAN_POINT ( 'NONE',  ( -3.749938752099124972, 0.02143258046192221891, 0.000000000000000000 ) ) ;
#5577 = CARTESIAN_POINT ( 'NONE',  ( 6.411082221499690093, -62.51743072077169217, -1.649542549651403789 ) ) ;
#5578 = VERTEX_POINT ( 'NONE', #6941 ) ;
#5579 = AXIS2_PLACEMENT_3D ( 'NONE', #7133, #1381, #3669 ) ;
#5580 = CIRCLE ( 'NONE', #407, 147.0000000000000000 ) ;
#5581 = CARTESIAN_POINT ( 'NONE',  ( 27.11783474234811564, -35.12923323413249221, -0.5000000000000350830 ) ) ;
#5582 = LINE ( 'NONE', #3190, #6061 ) ;
#5583 = VECTOR ( 'NONE', #4878, 1000.000000000000114 ) ;
#5584 = CARTESIAN_POINT ( 'NONE',  ( -3.498019654714389581, -55.03494779767484602, -0.2490962732230048438 ) ) ;
#5585 = VECTOR ( 'NONE', #1894, 1000.000000000000000 ) ;
#5586 = AXIS2_PLACEMENT_3D ( 'NONE', #3786, #2702, #2095 ) ;
#5587 = CIRCLE ( 'NONE', #7014, 0.9999999999999994449 ) ;
#5588 = FACE_OUTER_BOUND ( 'NONE', #3521, .T. ) ;
#5589 = CARTESIAN_POINT ( 'NONE',  ( -6.630541856184143157, -62.63987563302658401, 2.331428407641557676 ) ) ;
#5590 = EDGE_CURVE ( 'NONE', #6756, #577, #286, .T. ) ;
#5591 = EDGE_LOOP ( 'NONE', ( #4733, #7154 ) ) ;
#5592 = ADVANCED_BREP_SHAPE_REPRESENTATION ( '', ( #7333, #751 ), #6896 ) ;
#5593 = VECTOR ( 'NONE', #6160, 1000.000000000000000 ) ;
#5594 = STYLED_ITEM ( 'NONE', ( #6551 ), #7175 ) ;
#5595 = DIRECTION ( 'NONE',  ( -0.8795363392562568494, 0.4758317222797389667, 4.707970883985391064E-16 ) ) ;
#5596 = PLANE ( 'NONE',  #1003 ) ;
#5597 = DIRECTION ( 'NONE',  ( 0.3144019573014849023, -0.9492899500389726519, 0.000000000000000000 ) ) ;
#5598 = CARTESIAN_POINT ( 'NONE',  ( 6.071255580768259108, -56.77894568653594121, -1.427178034550365959 ) ) ;
#5599 = EDGE_CURVE ( 'NONE', #4842, #3938, #1256, .T. ) ;
#5600 = CARTESIAN_POINT ( 'NONE',  ( -12.11759654540111875, 13.15705282150456590, 3.000000000000012879 ) ) ;
#5601 = ORIENTED_EDGE ( 'NONE', *, *, #76, .T. ) ;
#5602 = CARTESIAN_POINT ( 'NONE',  ( -95.86211798318534250, -102.0316339954322018, -1.027823659516258203E-13 ) ) ;
#5603 = CARTESIAN_POINT ( 'NONE',  ( -12.11759654540111875, 13.15705282150456945, 1.301042606982605321E-14 ) ) ;
#5604 = CARTESIAN_POINT ( 'NONE',  ( -15.08175531864075047, -34.71610473016205134, -5.729623873133089518 ) ) ;
#5605 = CARTESIAN_POINT ( 'NONE',  ( -4.847093383240289377, -61.94486680083809205, -1.943810276119404046 ) ) ;
#5606 = CARTESIAN_POINT ( 'NONE',  ( 0.000000000000000000, 0.000000000000000000, -3.500000000000000000 ) ) ;
#5607 = EDGE_CURVE ( 'NONE', #1033, #7272, #1954, .T. ) ;
#5608 = CYLINDRICAL_SURFACE ( 'NONE', #2527, 5.000000000000000000 ) ;
#5609 = EDGE_CURVE ( 'NONE', #507, #909, #7374, .T. ) ;
#5610 = CARTESIAN_POINT ( 'NONE',  ( -5.010373352768399791, -62.05347898811812968, 1.680690861613699516 ) ) ;
#5611 = ORIENTED_EDGE ( 'NONE', *, *, #4125, .F. ) ;
#5612 = ORIENTED_EDGE ( 'NONE', *, *, #1023, .T. ) ;
#5613 = ORIENTED_EDGE ( 'NONE', *, *, #3784, .T. ) ;
#5614 = CARTESIAN_POINT ( 'NONE',  ( 0.000000000000000000, 0.000000000000000000, 0.000000000000000000 ) ) ;
#5615 = CARTESIAN_POINT ( 'NONE',  ( 28.22862315235815345, 26.16654680453439852, -0.8353469048621777748 ) ) ;
#5616 = ORIENTED_EDGE ( 'NONE', *, *, #3425, .F. ) ;
#5617 = DIRECTION ( 'NONE',  ( 0.9999836672264333925, -0.005715354789844381486, 0.000000000000000000 ) ) ;
#5618 = DIRECTION ( 'NONE',  ( -5.715354789860003484E-18, -9.999836672264337477E-16, 1.000000000000000000 ) ) ;
#5619 = DIRECTION ( 'NONE',  ( -0.6713653717954000122, 0.7411265327553888671, 8.673617379884183383E-16 ) ) ;
#5620 = CARTESIAN_POINT ( 'NONE',  ( 6.738276468386390050, -62.65933952543014129, -2.221138621355481568 ) ) ;
#5621 = ORIENTED_EDGE ( 'NONE', *, *, #4593, .F. ) ;
#5622 = CARTESIAN_POINT ( 'NONE',  ( -14.63712380658832046, -35.33334692323139592, -3.626931576674818025 ) ) ;
#5623 = CARTESIAN_POINT ( 'NONE',  ( 15.39900769062488806, 3.181283097128403625, 3.269241930315631824E-15 ) ) ;
#5624 = CARTESIAN_POINT ( 'NONE',  ( -17.64655212076966251, 14.06160472144369500, -1.351576240659936534 ) ) ;
#5625 = B_SPLINE_CURVE_WITH_KNOTS ( 'NONE', 3,
 ( #6518, #4758, #3825, #2526, #3051, #4876 ),
 .UNSPECIFIED., .F., .F.,
 ( 4, 2, 4 ),
 ( 0.000000000000000000, 0.0003937823932578689420, 0.0007875647865157378840 ),
 .UNSPECIFIED. ) ;
#5626 = DIRECTION ( 'NONE',  ( 0.3128463504745289114, 0.9445772445362836667, 0.09950371902099885979 ) ) ;
#5627 = CARTESIAN_POINT ( 'NONE',  ( -6.535529569156460106, -62.60774289024404027, 2.066694991760122502 ) ) ;
#5628 = ORIENTED_EDGE ( 'NONE', *, *, #588, .T. ) ;
#5629 = CARTESIAN_POINT ( 'NONE',  ( 44.95353084483765826, -94.82378791335750634, -9.454242944073598665E-14 ) ) ;
#5630 = FACE_OUTER_BOUND ( 'NONE', #3983, .T. ) ;
#5631 = DIRECTION ( 'NONE',  ( 0.6513146796332662802, 0.5900073775824580258, -0.4771587602596085720 ) ) ;
#5632 = CARTESIAN_POINT ( 'NONE',  ( -5.788105944719140084, -64.22553544194731501, 1.709038299673605321 ) ) ;
#5633 = DIRECTION ( 'NONE',  ( 0.9999836672264332815, -0.005715354789860000936, 0.000000000000000000 ) ) ;
#5634 = ORIENTED_EDGE ( 'NONE', *, *, #1994, .F. ) ;
#5635 = ORIENTED_EDGE ( 'NONE', *, *, #5430, .T. ) ;
#5636 = CARTESIAN_POINT ( 'NONE',  ( 2.303277369485650095, -64.96541665026637702, 1.677260903589945285 ) ) ;
#5637 = EDGE_CURVE ( 'NONE', #3224, #1441, #1749, .T. ) ;
#5638 = DIRECTION ( 'NONE',  ( 0.9999836672264331705, -0.005715354789862803382, 0.000000000000000000 ) ) ;
#5639 = DIRECTION ( 'NONE',  ( -5.715354789845005112E-18, -9.999836672264339449E-16, 1.000000000000000000 ) ) ;
#5640 = CARTESIAN_POINT ( 'NONE',  ( -4.596296085628660322, -63.12536419624139938, 1.105086706205665070 ) ) ;
#5641 = DIRECTION ( 'NONE',  ( 0.8688689365825388311, 0.4950421911735690128, 0.000000000000000000 ) ) ;
#5642 = DIRECTION ( 'NONE',  ( 0.000000000000000000, 0.000000000000000000, -1.000000000000000000 ) ) ;
#5643 = VERTEX_POINT ( 'NONE', #2897 ) ;
#5644 = ORIENTED_EDGE ( 'NONE', *, *, #5701, .T. ) ;
#5645 = ORIENTED_EDGE ( 'NONE', *, *, #2071, .F. ) ;
#5646 = ADVANCED_FACE ( 'NONE', ( #655 ), #5348, .F. ) ;
#5647 = ADVANCED_FACE ( 'NONE', ( #1815 ), #5824, .T. ) ;
#5648 = ORIENTED_EDGE ( 'NONE', *, *, #7295, .F. ) ;
#5649 = CARTESIAN_POINT ( 'NONE',  ( -10.54744521951312208, -8.271218886098244738, -3.000000000000009326 ) ) ;
#5650 = DIRECTION ( 'NONE',  ( 0.000000000000000000, 0.000000000000000000, -1.000000000000000000 ) ) ;
#5651 = CARTESIAN_POINT ( 'NONE',  ( 2.082020516433249924, -53.40759131075155608, 1.446381639928540297 ) ) ;
#5652 = ORIENTED_EDGE ( 'NONE', *, *, #1669, .T. ) ;
#5653 = FACE_OUTER_BOUND ( 'NONE', #482, .T. ) ;
#5654 = EDGE_CURVE ( 'NONE', #1522, #4585, #5713, .T. ) ;
#5655 = CARTESIAN_POINT ( 'NONE',  ( -5.794328821513979655, -59.26142744441108334, -0.3953236866292048068 ) ) ;
#5656 = CARTESIAN_POINT ( 'NONE',  ( 19.86817077757007510, -41.71399671145088917, -3.001370543551582060 ) ) ;
#5657 = CIRCLE ( 'NONE', #1800, 140.0000000000000000 ) ;
#5658 = DIRECTION ( 'NONE',  ( 5.715354789845005112E-18, 9.999836672264339449E-16, -1.000000000000000000 ) ) ;
#5659 = LINE ( 'NONE', #6775, #5183 ) ;
#5660 = ORIENTED_EDGE ( 'NONE', *, *, #979, .F. ) ;
#5661 = VECTOR ( 'NONE', #2968, 999.9999999999998863 ) ;
#5662 = EDGE_CURVE ( 'NONE', #5081, #7087, #3411, .T. ) ;
#5663 = CYLINDRICAL_SURFACE ( 'NONE', #5930, 0.9999999999999988898 ) ;
#5664 = FACE_OUTER_BOUND ( 'NONE', #1892, .T. ) ;
#5665 = LINE ( 'NONE', #5058, #3715 ) ;
#5666 =( GEOMETRIC_REPRESENTATION_CONTEXT ( 3 ) GLOBAL_UNCERTAINTY_ASSIGNED_CONTEXT ( ( #722 ) ) GLOBAL_UNIT_ASSIGNED_CONTEXT ( ( #4037, #602, #6338 ) ) REPRESENTATION_CONTEXT ( 'NONE', 'WORKASPACE' ) );
#5667 = CARTESIAN_POINT ( 'NONE',  ( -6.519675230953620115, -62.56018929471859735, 1.797154853076760261 ) ) ;
#5668 = PLANE ( 'NONE',  #6193 ) ;
#5669 = ORIENTED_EDGE ( 'NONE', *, *, #5554, .F. ) ;
#5670 = DIRECTION ( 'NONE',  ( -5.715354789845005112E-18, -9.999836672264339449E-16, 1.000000000000000000 ) ) ;
#5671 = CARTESIAN_POINT ( 'NONE',  ( 4.230506805399654624, -63.24565307424497007, 1.502053860026275167 ) ) ;
#5672 = VECTOR ( 'NONE', #4681, 1000.000000000000000 ) ;
#5673 = CARTESIAN_POINT ( 'NONE',  ( 15.08188723176695056, -34.71618050577090031, 5.760870465243799643 ) ) ;
#5674 = DIRECTION ( 'NONE',  ( 0.3213584079436493934, -0.3547505615521249767, 0.8779981849197495691 ) ) ;
#5675 = CARTESIAN_POINT ( 'NONE',  ( -4.653276882800380321, -62.74377975942224595, 3.226317067983300202 ) ) ;
#5676 = CARTESIAN_POINT ( 'NONE',  ( 27.23276465633407284, -35.06523870642838858, 3.999999999999965361 ) ) ;
#5677 = CARTESIAN_POINT ( 'NONE',  ( 2.420475147787775505, -66.32055832903793657, -1.240572518232158972 ) ) ;
#5678 = ORIENTED_EDGE ( 'NONE', *, *, #2930, .F. ) ;
#5679 = EDGE_CURVE ( 'NONE', #937, #6339, #5895, .T. ) ;
#5680 = VERTEX_POINT ( 'NONE', #6481 ) ;
#5681 = ORIENTED_EDGE ( 'NONE', *, *, #1775, .T. ) ;
#5682 = ITEM_DEFINED_TRANSFORMATION ( 'NONE', 'NONE', #5586,  #751 ) ;
#5683 = DIRECTION ( 'NONE',  ( -0.3866393274467394559, 0.9222310071080526139, 9.200061635857666883E-16 ) ) ;
#5684 = ORIENTED_EDGE ( 'NONE', *, *, #7327, .T. ) ;
#5685 = CIRCLE ( 'NONE', #622, 3.299999999999999822 ) ;
#5686 = DIRECTION ( 'NONE',  ( 0.9999836672264331705, -0.005715354789862803382, 0.000000000000000000 ) ) ;
#5687 = LINE ( 'NONE', #5126, #3631 ) ;
#5688 = CARTESIAN_POINT ( 'NONE',  ( 3.914764119449064772, -54.23824460091720567, 1.533423736523834346 ) ) ;
#5689 = EDGE_CURVE ( 'NONE', #123, #5269, #7259, .T. ) ;
#5690 = EDGE_CURVE ( 'NONE', #6854, #3586, #6908, .T. ) ;
#5691 = VECTOR ( 'NONE', #2957, 1000.000000000000114 ) ;
#5692 = VECTOR ( 'NONE', #1993, 1000.000000000000114 ) ;
#5693 = CARTESIAN_POINT ( 'NONE',  ( 8.554393258638587128, 16.61373401801076000, -0.1388209971588536540 ) ) ;
#5694 = CARTESIAN_POINT ( 'NONE',  ( -32.59768532061907109, 15.27050393970921327, -1.493845543551520327 ) ) ;
#5695 = VECTOR ( 'NONE', #3, 1000.000000000000000 ) ;
#5696 = DIRECTION ( 'NONE',  ( -5.715354789845005112E-18, -9.999836672264339449E-16, 1.000000000000000000 ) ) ;
#5697 = VECTOR ( 'NONE', #2289, 1000.000000000000000 ) ;
#5698 = DIRECTION ( 'NONE',  ( -5.715354789860003484E-18, -9.999836672264337477E-16, 1.000000000000000000 ) ) ;
#5699 = SURFACE_SIDE_STYLE ('',( #6963 ) ) ;
#5700 = CIRCLE ( 'NONE', #1597, 1.000000000000000444 ) ;
#5701 = EDGE_CURVE ( 'NONE', #6909, #2342, #1372, .T. ) ;
#5702 = EDGE_CURVE ( 'NONE', #181, #1973, #3688, .T. ) ;
#5703 = VERTEX_POINT ( 'NONE', #2528 ) ;
#5704 = VECTOR ( 'NONE', #6571, 999.9999999999998863 ) ;
#5705 = AXIS2_PLACEMENT_3D ( 'NONE', #1722, #7401, #1122 ) ;
#5706 = AXIS2_PLACEMENT_3D ( 'NONE', #5077, #6217, #1011 ) ;
#5707 = CARTESIAN_POINT ( 'NONE',  ( 18.06432742338256148, -39.71205111763084972, 3.065817211669312314 ) ) ;
#5708 = DIRECTION ( 'NONE',  ( 0.000000000000000000, -0.7252565289002705917, -0.6884787340851793447 ) ) ;
#5709 = DIRECTION ( 'NONE',  ( -0.9793199139485100346, -0.2023178344681531293, -1.787644449902631965E-16 ) ) ;
#5710 = CARTESIAN_POINT ( 'NONE',  ( -3.268733238405740149, -66.73531384189965365, -2.665188268689791862 ) ) ;
#5711 = LINE ( 'NONE', #4457, #7226 ) ;
#5712 = EDGE_CURVE ( 'NONE', #5715, #1992, #4833, .T. ) ;
#5713 = CIRCLE ( 'NONE', #6660, 1.100000000000000755 ) ;
#5714 = VECTOR ( 'NONE', #1241, 999.9999999999998863 ) ;
#5715 = VERTEX_POINT ( 'NONE', #5325 ) ;
#5716 = CARTESIAN_POINT ( 'NONE',  ( -105.7473861751082040, -118.0666774205683822, -1.188285581044112860E-13 ) ) ;
#5717 = CARTESIAN_POINT ( 'NONE',  ( 17.99681370199822439, -40.34754878873740580, -0.5037687939243526980 ) ) ;
#5718 = VECTOR ( 'NONE', #3164, 1000.000000000000227 ) ;
#5719 = CARTESIAN_POINT ( 'NONE',  ( -13.49899450467539985, -35.75040780681265318, -2.566271404894997499 ) ) ;
#5720 = CARTESIAN_POINT ( 'NONE',  ( -2.437747074861595031, -55.99259917890189797, 0.6173017669495700632 ) ) ;
#5721 = FACE_OUTER_BOUND ( 'NONE', #929, .T. ) ;
#5722 = DIRECTION ( 'NONE',  ( -0.4039838799357176602, -0.9147661038495489283, -9.170600743851254660E-16 ) ) ;
#5723 = ORIENTED_EDGE ( 'NONE', *, *, #5222, .T. ) ;
#5724 = ORIENTED_EDGE ( 'NONE', *, *, #1767, .T. ) ;
#5725 = EDGE_LOOP ( 'NONE', ( #6095, #792, #7307, #97 ) ) ;
#5726 = ORIENTED_EDGE ( 'NONE', *, *, #5872, .F. ) ;
#5727 = PRODUCT_CONTEXT ( 'NONE', #6027, 'mechanical' ) ;
#5728 = DIRECTION ( 'NONE',  ( -0.9986925448795970217, -0.05111947575938272093, -5.682652305652042775E-17 ) ) ;
#5729 = ORIENTED_EDGE ( 'NONE', *, *, #1901, .F. ) ;
#5730 = EDGE_CURVE ( 'NONE', #5520, #6609, #867, .T. ) ;
#5731 = DIRECTION ( 'NONE',  ( 0.9999836672264332815, -0.005715354789845306094, 0.000000000000000000 ) ) ;
#5732 = DIRECTION ( 'NONE',  ( 0.7411265327553895332, 0.6713653717953992350, 1.304512053934558935E-15 ) ) ;
#5733 = SPHERICAL_SURFACE ( 'NONE', #2803, 7.844444444444450326 ) ;
#5734 = CARTESIAN_POINT ( 'NONE',  ( -6.840816475388580287, -61.57127885238590892, 1.848044054229609934 ) ) ;
#5735 = DIRECTION ( 'NONE',  ( -0.6713653717954000122, 0.7411265327553888671, 8.673617379884183383E-16 ) ) ;
#5736 = CARTESIAN_POINT ( 'NONE',  ( 27.55794480445177541, -34.88416442371428161, -0.8737476923743859869 ) ) ;
#5737 = DIRECTION ( 'NONE',  ( 0.3309668111461608886, 0.9436423951475163552, 9.455185755993174392E-16 ) ) ;
#5738 = ADVANCED_FACE ( 'NONE', ( #2571 ), #7118, .T. ) ;
#5739 = CARTESIAN_POINT ( 'NONE',  ( 20.29543457672885154, -41.45429371584161515, -3.001370543551582060 ) ) ;
#5740 = DIRECTION ( 'NONE',  ( -0.9999836672264333925, 0.005715354789844971292, -3.141587852546554631E-32 ) ) ;
#5741 = EDGE_CURVE ( 'NONE', #7211, #5434, #3420, .T. ) ;
#5742 = CARTESIAN_POINT ( 'NONE',  ( 17.61082885536508158, -39.97043407431674922, 3.134598002289771923 ) ) ;
#5743 = EDGE_CURVE ( 'NONE', #555, #1354, #2574, .T. ) ;
#5744 = CARTESIAN_POINT ( 'NONE',  ( -12.11759654540111875, 13.15705282150456945, 1.301042606982605321E-14 ) ) ;
#5745 = DIRECTION ( 'NONE',  ( 0.2223191033124283789, 0.6712482523644727195, 0.7071067811865466846 ) ) ;
#5746 = CARTESIAN_POINT ( 'NONE',  ( -6.921793923077749433, -58.90709844370859116, -2.222636374480685184 ) ) ;
#5747 = DIRECTION ( 'NONE',  ( 5.715354789845005112E-18, 9.999836672264339449E-16, -1.000000000000000000 ) ) ;
#5748 = ORIENTED_EDGE ( 'NONE', *, *, #7190, .F. ) ;
#5749 = CARTESIAN_POINT ( 'NONE',  ( -4.860610968486169803, -1.172374092613760022, -3.000000000000000000 ) ) ;
#5750 = FACE_OUTER_BOUND ( 'NONE', #434, .T. ) ;
#5751 = CARTESIAN_POINT ( 'NONE',  ( 26.87031364676134970, -34.69479876584121314, 3.499999999999965361 ) ) ;
#5752 = DIRECTION ( 'NONE',  ( 0.7411265327553895332, 0.6713653717953993461, 1.302304562955136699E-15 ) ) ;
#5753 = CARTESIAN_POINT ( 'NONE',  ( -3.222464925939095171, -55.48519077065235194, -0.1302151132178846482 ) ) ;
#5754 = DIRECTION ( 'NONE',  ( 0.9999836672264333925, -0.005715354789844381486, 0.000000000000000000 ) ) ;
#5755 = DIRECTION ( 'NONE',  ( 2.857391495672265093E-16, 4.793132013414519254E-17, 1.000000000000000000 ) ) ;
#5756 = ORIENTED_EDGE ( 'NONE', *, *, #3822, .T. ) ;
#5757 = ORIENTED_EDGE ( 'NONE', *, *, #7284, .F. ) ;
#5758 = ORIENTED_EDGE ( 'NONE', *, *, #1343, .F. ) ;
#5759 = CONTEXT_DEPENDENT_SHAPE_REPRESENTATION ( #99, #6043 ) ;
#5760 = CARTESIAN_POINT ( 'NONE',  ( -34.88460058024266175, 16.28046363954879183, -0.7438455435519999437 ) ) ;
#5761 = ADVANCED_FACE ( 'NONE', ( #3660 ), #795, .F. ) ;
#5762 = CARTESIAN_POINT ( 'NONE',  ( -18.46249958194447771, 2.687629333967654244, -0.3999035282155169457 ) ) ;
#5763 = CARTESIAN_POINT ( 'NONE',  ( 1.211170193666210038, -66.82801115824167937, 0.9562527914032201704 ) ) ;
#5764 = CARTESIAN_POINT ( 'NONE',  ( 26.87031364676133194, -34.69479876584122024, -1.000000000000034861 ) ) ;
#5765 = CARTESIAN_POINT ( 'NONE',  ( -2.876828494605734754, -55.82398600891924190, -2.074803592940099861 ) ) ;
#5766 = VERTEX_POINT ( 'NONE', #236 ) ;
#5767 = EDGE_LOOP ( 'NONE', ( #7165, #1583, #1146, #6429, #4004, #1171, #7356, #2854, #5416, #2566, #4046, #4277, #7388, #4242, #4927, #7402, #7046, #114, #4804, #6955, #2038, #1541, #1048, #4433, #6837, #3367, #1769, #3092, #3625, #2468, #1337, #772, #3414 ) ) ;
#5768 = EDGE_LOOP ( 'NONE', ( #1768, #2610, #4829, #3135 ) ) ;
#5769 = CARTESIAN_POINT ( 'NONE',  ( -1.172374092613760022, 4.860610968486169803, 3.500000000000000000 ) ) ;
#5770 = CARTESIAN_POINT ( 'NONE',  ( -31.91091272472834817, 16.82560631625344172, -2.993845543551523214 ) ) ;
#5771 = CARTESIAN_POINT ( 'NONE',  ( 15.49911764349215026, -35.75048010860329839, 2.597518595105000383 ) ) ;
#5772 = CYLINDRICAL_SURFACE ( 'NONE', #2196, 0.7500000000000003331 ) ;
#5773 = CARTESIAN_POINT ( 'NONE',  ( 27.11783474234813340, -35.12923323413248511, 3.999999999999965361 ) ) ;
#5774 = DIRECTION ( 'NONE',  ( 0.9571808262218332031, -0.2894907009098718897, -1.790426255900482524E-16 ) ) ;
#5775 = ORIENTED_EDGE ( 'NONE', *, *, #1362, .T. ) ;
#5776 = ADVANCED_FACE ( 'NONE', ( #4304 ), #1885, .T. ) ;
#5777 = DIRECTION ( 'NONE',  ( -0.4039838799357192700, -0.9147661038495482622, -8.673617379884158732E-16 ) ) ;
#5778 = CARTESIAN_POINT ( 'NONE',  ( 17.88843813672053074, -40.41242482140540204, -4.025211077939831437E-14 ) ) ;
#5779 = CARTESIAN_POINT ( 'NONE',  ( 1.791628076902189504, -65.99651092193212776, 1.035779542278230991 ) ) ;
#5780 = CARTESIAN_POINT ( 'NONE',  ( 5.575556491096470779, -57.10417477796837460, -1.782215851858570010 ) ) ;
#5781 = CARTESIAN_POINT ( 'NONE',  ( 104.0973215944787711, -119.5240462704291389, -3.000000000000119904 ) ) ;
#5782 = CIRCLE ( 'NONE', #6972, 145.9999999999999716 ) ;
#5783 = VERTEX_POINT ( 'NONE', #165 ) ;
#5784 = EDGE_CURVE ( 'NONE', #2318, #4359, #6045, .T. ) ;
#5785 = FACE_OUTER_BOUND ( 'NONE', #1196, .T. ) ;
#5786 = CYLINDRICAL_SURFACE ( 'NONE', #417, 147.0000000000000000 ) ;
#5787 = LINE ( 'NONE', #1072, #4857 ) ;
#5788 = VECTOR ( 'NONE', #4377, 1000.000000000000000 ) ;
#5789 = DIRECTION ( 'NONE',  ( 0.9147661038495520369, -0.4039838799357104437, -5.652825226190241484E-16 ) ) ;
#5790 = CARTESIAN_POINT ( 'NONE',  ( 4.514859508800350696, -57.62591736726079006, 0.04509635899271501047 ) ) ;
#5791 = LINE ( 'NONE', #17, #5937 ) ;
#5792 = DIRECTION ( 'NONE',  ( -0.5224671166576538850, 0.8526594349512809368, 0.000000000000000000 ) ) ;
#5793 = ORIENTED_EDGE ( 'NONE', *, *, #3932, .F. ) ;
#5794 = ORIENTED_EDGE ( 'NONE', *, *, #5045, .T. ) ;
#5795 = EDGE_CURVE ( 'NONE', #123, #3009, #2452, .T. ) ;
#5796 = ORIENTED_EDGE ( 'NONE', *, *, #4767, .F. ) ;
#5797 = ORIENTED_EDGE ( 'NONE', *, *, #1986, .T. ) ;
#5798 = VECTOR ( 'NONE', #5230, 1000.000000000000114 ) ;
#5799 = CARTESIAN_POINT ( 'NONE',  ( -15.02360761328580097, -37.34705832593169816, 1.026284428608169819 ) ) ;
#5800 = ORIENTED_EDGE ( 'NONE', *, *, #175, .T. ) ;
#5801 = CARTESIAN_POINT ( 'NONE',  ( 27.98760434640042050, 26.43260972569849443, -1.493845543551990174 ) ) ;
#5802 = CARTESIAN_POINT ( 'NONE',  ( -3.697637789055789881, -65.78881948023087034, 1.221121406208630411 ) ) ;
#5803 = CIRCLE ( 'NONE', #2535, 2.499999999999997335 ) ;
#5804 = CARTESIAN_POINT ( 'NONE',  ( 27.81599406684724229, -34.74046346518214534, -0.6152221228502958716 ) ) ;
#5805 = CARTESIAN_POINT ( 'NONE',  ( -1.110895189285712181, -65.77251424999820983, -2.870029284013874360 ) ) ;
#5806 = ADVANCED_FACE ( 'NONE', ( #4188 ), #6197, .T. ) ;
#5807 = VERTEX_POINT ( 'NONE', #7412 ) ;
#5808 = SURFACE_STYLE_USAGE ( .BOTH. , #4032 ) ;
#5809 = FACE_OUTER_BOUND ( 'NONE', #219, .T. ) ;
#5810 = CYLINDRICAL_SURFACE ( 'NONE', #2344, 0.7500000000000003331 ) ;
#5811 = DIRECTION ( 'NONE',  ( -5.715354789845005112E-18, -9.999836672264339449E-16, 1.000000000000000000 ) ) ;
#5812 = DIRECTION ( 'NONE',  ( 5.715354789845005112E-18, 9.999836672264339449E-16, -1.000000000000000000 ) ) ;
#5813 = DIRECTION ( 'NONE',  ( 0.6778072752560848624, -0.7352396191786197965, -6.263809825053043546E-16 ) ) ;
#5814 = AXIS2_PLACEMENT_3D ( 'NONE', #2068, #4337, #2637 ) ;
#5815 = AXIS2_PLACEMENT_3D ( 'NONE', #4482, #7329, #3863 ) ;
#5816 = PRESENTATION_LAYER_ASSIGNMENT (  '', '', ( #1833 ) ) ;
#5817 = CARTESIAN_POINT ( 'NONE',  ( -2.864422359069719981, -64.63427441546140528, 2.032225693688770374 ) ) ;
#5818 = AXIS2_PLACEMENT_3D ( 'NONE', #3422, #4064, #4601 ) ;
#5819 = SURFACE_SIDE_STYLE ('',( #1359 ) ) ;
#5820 = CIRCLE ( 'NONE', #1123, 141.0000000000000284 ) ;
#5821 = DIRECTION ( 'NONE',  ( 3.410558963702386264E-15, 4.255734876089061273E-15, -1.000000000000000000 ) ) ;
#5822 = DIRECTION ( 'NONE',  ( 0.2223157560262039867, -0.6712493609847990372, 0.7071067811865450192 ) ) ;
#5823 = CARTESIAN_POINT ( 'NONE',  ( 5.766865232587130130, -57.44905037028758699, 0.3380538640060152256 ) ) ;
#5824 = CYLINDRICAL_SURFACE ( 'NONE', #4259, 1.000000000000000888 ) ;
#5825 = VECTOR ( 'NONE', #3892, 1000.000000000000114 ) ;
#5826 = AXIS2_PLACEMENT_3D ( 'NONE', #3255, #7177, #410 ) ;
#5827 = VERTEX_POINT ( 'NONE', #5771 ) ;
#5828 = CARTESIAN_POINT ( 'NONE',  ( -5.219056089447164481, -62.17188307074363962, 3.392373891847805467 ) ) ;
#5829 = DIRECTION ( 'NONE',  ( -5.715354789845005112E-18, -9.999836672264339449E-16, 1.000000000000000000 ) ) ;
#5830 = CIRCLE ( 'NONE', #3160, 0.5000000000000004441 ) ;
#5831 = VECTOR ( 'NONE', #6825, 1000.000000000000114 ) ;
#5832 = DIRECTION ( 'NONE',  ( 0.000000000000000000, 0.000000000000000000, 1.000000000000000000 ) ) ;
#5833 = ADVANCED_FACE ( 'NONE', ( #912 ), #346, .F. ) ;
#5834 = CARTESIAN_POINT ( 'NONE',  ( -4.908132910216119527, -63.74296424117085991, -0.6604057789239049514 ) ) ;
#5835 = CIRCLE ( 'NONE', #5105, 6.500000000000001776 ) ;
#5836 = VECTOR ( 'NONE', #1288, 1000.000000000000000 ) ;
#5837 = CARTESIAN_POINT ( 'NONE',  ( 6.187144687173720570, -58.64655194120005177, 0.3691021985165400809 ) ) ;
#5838 = DIRECTION ( 'NONE',  ( 0.9999836672264332815, -0.005715354789860000936, 0.000000000000000000 ) ) ;
#5839 = PRODUCT_RELATED_PRODUCT_CATEGORY ( 'part', '', ( #6392 ) ) ;
#5840 = VERTEX_POINT ( 'NONE', #6811 ) ;
#5841 = ORIENTED_EDGE ( 'NONE', *, *, #5679, .F. ) ;
#5842 = VERTEX_POINT ( 'NONE', #3950 ) ;
#5843 = TOROIDAL_SURFACE ( 'NONE', #2811, 2.249999999999964917, 1.000000000000000000 ) ;
#5844 = CARTESIAN_POINT ( 'NONE',  ( -33.94153943842304955, 12.25650441806195801, -2.999999999999988898 ) ) ;
#5845 = DIRECTION ( 'NONE',  ( -0.3536350175650626038, -0.3203478684871197690, -0.8788171126619672702 ) ) ;
#5846 = EDGE_CURVE ( 'NONE', #1231, #420, #533, .T. ) ;
#5847 = EDGE_CURVE ( 'NONE', #2318, #6014, #6258, .T. ) ;
#5848 = CARTESIAN_POINT ( 'NONE',  ( -3.648210298237669846, -66.52323838441711246, -0.5446899798612400145 ) ) ;
#5849 = CYLINDRICAL_SURFACE ( 'NONE', #2063, 0.9999999999999984457 ) ;
#5850 = ORIENTED_EDGE ( 'NONE', *, *, #6829, .F. ) ;
#5851 = AXIS2_PLACEMENT_3D ( 'NONE', #7256, #297, #4405 ) ;
#5852 = EDGE_LOOP ( 'NONE', ( #2231, #2313, #7441, #877 ) ) ;
#5853 = LINE ( 'NONE', #5770, #150 ) ;
#5854 = EDGE_CURVE ( 'NONE', #4023, #321, #7229, .T. ) ;
#5855 = CARTESIAN_POINT ( 'NONE',  ( 6.588013489872674988, -62.64654932776589646, -2.867023156876145507 ) ) ;
#5856 = CARTESIAN_POINT ( 'NONE',  ( -5.524241737545620090, -57.12730840725460979, 1.694319224817255165 ) ) ;
#5857 = CARTESIAN_POINT ( 'NONE',  ( 4.469984187763964556, -63.33186444122004843, 2.519959534738519746 ) ) ;
#5858 = PRESENTATION_STYLE_ASSIGNMENT (( #51 ) ) ;
#5859 = CYLINDRICAL_SURFACE ( 'NONE', #4807, 0.9999999999999991118 ) ;
#5860 = CARTESIAN_POINT ( 'NONE',  ( -0.9067045181355430916, -66.16172987439199460, 1.193114471962507972 ) ) ;
#5861 = EDGE_LOOP ( 'NONE', ( #4016, #3310 ) ) ;
#5862 = CARTESIAN_POINT ( 'NONE',  ( -28.02385480137132845, 13.25058454003066188, -1.493845543551522104 ) ) ;
#5863 = CARTESIAN_POINT ( 'NONE',  ( 27.09755250833208606, -34.56532834836465895, 3.445680074011886251 ) ) ;
#5864 = CARTESIAN_POINT ( 'NONE',  ( 18.38473276620558750, -39.52949865626803927, -0.4867457206136995285 ) ) ;
#5865 = PRODUCT_DEFINITION_CONTEXT ( 'detailed design', #2933, 'design' ) ;
#5866 = CARTESIAN_POINT ( 'NONE',  ( -5.710866809226770258, -58.90547762198222870, 1.725351541085619500 ) ) ;
#5867 = CARTESIAN_POINT ( 'NONE',  ( 6.265638173095489982, -61.94185186372677521, 0.5461908750427398873 ) ) ;
#5868 = DIRECTION ( 'NONE',  ( 2.857391495672265093E-16, 4.793132013414519254E-17, 1.000000000000000000 ) ) ;
#5869 = ORIENTED_EDGE ( 'NONE', *, *, #2894, .F. ) ;
#5870 = ORIENTED_EDGE ( 'NONE', *, *, #310, .F. ) ;
#5871 = ORIENTED_EDGE ( 'NONE', *, *, #2466, .F. ) ;
#5872 = EDGE_CURVE ( 'NONE', #6679, #5807, #176, .T. ) ;
#5873 = CARTESIAN_POINT ( 'NONE',  ( 24.99346688245966419, 26.01411140189437532, -2.993845543551503674 ) ) ;
#5874 = FACE_OUTER_BOUND ( 'NONE', #3029, .T. ) ;
#5875 = CARTESIAN_POINT ( 'NONE',  ( -3.079777581550224852, -54.72070545288789134, -0.1918259013367045740 ) ) ;
#5876 = LINE ( 'NONE', #2845, #3412 ) ;
#5877 = EDGE_LOOP ( 'NONE', ( #5902, #5903, #701, #5406, #4325, #3101 ) ) ;
#5878 = ORIENTED_EDGE ( 'NONE', *, *, #7380, .F. ) ;
#5879 = ADVANCED_FACE ( 'NONE', ( #4034 ), #3765, .F. ) ;
#5880 = ADVANCED_FACE ( 'NONE', ( #3199 ), #2638, .T. ) ;
#5881 = PLANE ( 'NONE',  #3750 ) ;
#5882 = CARTESIAN_POINT ( 'NONE',  ( -13.60410507457170226, -35.67283034916086848, -3.000000000000036415 ) ) ;
#5883 = FACE_OUTER_BOUND ( 'NONE', #1564, .T. ) ;
#5884 = CARTESIAN_POINT ( 'NONE',  ( 2.986904076224405014, -66.15109244657664078, 2.931604786918900363 ) ) ;
#5885 = CARTESIAN_POINT ( 'NONE',  ( 4.371277347803607327, -55.97928041872565785, 2.299471528649866148 ) ) ;
#5886 = EDGE_CURVE ( 'NONE', #1686, #3635, #1147, .T. ) ;
#5887 = CARTESIAN_POINT ( 'NONE',  ( -4.716938577623720263, -57.97996379370297149, -0.6608593144672147979 ) ) ;
#5888 = CARTESIAN_POINT ( 'NONE',  ( 44.95353084483765826, -94.82378791335750634, 2.999999999999905409 ) ) ;
#5889 = CARTESIAN_POINT ( 'NONE',  ( 4.748085323256989732, -62.01668842780453872, -2.502390571778199568 ) ) ;
#5890 = CARTESIAN_POINT ( 'NONE',  ( -4.425770051009331851, -64.17614344307862950, -0.6687802702403959909 ) ) ;
#5891 = DIRECTION ( 'NONE',  ( 0.4039838799357100552, 0.9147661038495522590, 1.626385516829955012E-16 ) ) ;
#5892 = VERTEX_POINT ( 'NONE', #2256 ) ;
#5893 = CARTESIAN_POINT ( 'NONE',  ( 13.61290835672744848, 19.61678186576282812, 0.1446417891851695114 ) ) ;
#5894 = CIRCLE ( 'NONE', #352, 11.50000000000000178 ) ;
#5895 = LINE ( 'NONE', #6521, #3044 ) ;
#5896 = CARTESIAN_POINT ( 'NONE',  ( 18.38461951018646445, -39.52956318442134886, -1.002819413936762105 ) ) ;
#5897 = CARTESIAN_POINT ( 'NONE',  ( -5.211262431554310126, -59.36811747016641050, -0.7503612693867500738 ) ) ;
#5898 = VECTOR ( 'NONE', #4447, 1000.000000000000114 ) ;
#5899 = CARTESIAN_POINT ( 'NONE',  ( 6.162074140922939591, -62.32076522084695114, 2.666565443060120444 ) ) ;
#5900 = FACE_BOUND ( 'NONE', #853, .T. ) ;
#5901 = ORIENTED_EDGE ( 'NONE', *, *, #4707, .F. ) ;
#5902 = ORIENTED_EDGE ( 'NONE', *, *, #2873, .F. ) ;
#5903 = ORIENTED_EDGE ( 'NONE', *, *, #7382, .T. ) ;
#5904 = ORIENTED_EDGE ( 'NONE', *, *, #5590, .F. ) ;
#5905 = FACE_OUTER_BOUND ( 'NONE', #4779, .T. ) ;
#5906 = LINE ( 'NONE', #731, #2793 ) ;
#5907 = CARTESIAN_POINT ( 'NONE',  ( -5.727966693761760375, -63.15494832584334262, 1.398024598501910187 ) ) ;
#5908 = DIRECTION ( 'NONE',  ( 0.000000000000000000, 1.000000000000000000, 1.734723475976805517E-15 ) ) ;
#5909 = EDGE_CURVE ( 'NONE', #4166, #7056, #1058, .T. ) ;
#5910 = ORIENTED_EDGE ( 'NONE', *, *, #3652, .F. ) ;
#5911 = AXIS2_PLACEMENT_3D ( 'NONE', #917, #800, #5495 ) ;
#5912 = ORIENTED_EDGE ( 'NONE', *, *, #77, .T. ) ;
#5913 = CARTESIAN_POINT ( 'NONE',  ( 37.86567095459282228, 7.005780695865149177, -1.500000000001998623 ) ) ;
#5914 = DIRECTION ( 'NONE',  ( 0.000000000000000000, 0.000000000000000000, 1.000000000000000000 ) ) ;
#5915 = CARTESIAN_POINT ( 'NONE',  ( 39.48483786921892857, -95.33781693134928048, -9.519295074422728931E-14 ) ) ;
#5916 = DIRECTION ( 'NONE',  ( -5.715354789860003484E-18, -9.999836672264337477E-16, 1.000000000000000000 ) ) ;
#5917 = EDGE_CURVE ( 'NONE', #7060, #5520, #3347, .T. ) ;
#5918 = CARTESIAN_POINT ( 'NONE',  ( 43.95483829995806957, -94.87490738911687060, -1.000000000000094591 ) ) ;
#5919 = EDGE_CURVE ( 'NONE', #6558, #3357, #2092, .T. ) ;
#5920 = VERTEX_POINT ( 'NONE', #5134 ) ;
#5921 = CLOSED_SHELL ( 'NONE', ( #3874, #5553, #6560, #1083, #4485, #4972, #7062, #7145, #4039, #5974, #6515, #5738, #6700, #319, #6329, #847, #2224, #3315, #6507, #2465, #1632, #3565, #5290, #6249, #1851, #6779, #5761, #4431, #4105, #7392, #5176, #2825, #2129, #6343, #6272, #1788, #3528, #2856, #3379, #4017, #7202, #3557 ) ) ;
#5922 = CARTESIAN_POINT ( 'NONE',  ( -5.135436550704829628, -59.04801135763068487, 1.370314102932454814 ) ) ;
#5923 = FACE_OUTER_BOUND ( 'NONE', #2644, .T. ) ;
#5924 = DIRECTION ( 'NONE',  ( 0.9147661038495520369, -0.4039838799357104437, -5.652825226190241484E-16 ) ) ;
#5925 = EDGE_CURVE ( 'NONE', #6624, #4278, #1736, .T. ) ;
#5926 = ADVANCED_FACE ( 'NONE', ( #4528 ), #7263, .F. ) ;
#5927 = CARTESIAN_POINT ( 'NONE',  ( -5.562592810569134905, -62.20808427580125510, -0.5376115902277359693 ) ) ;
#5928 = CARTESIAN_POINT ( 'NONE',  ( -1.409024882572649906, -54.10038288851608712, -0.1041033434293599513 ) ) ;
#5929 = ORIENTED_EDGE ( 'NONE', *, *, #1650, .T. ) ;
#5930 = AXIS2_PLACEMENT_3D ( 'NONE', #1658, #4609, #6739 ) ;
#5931 = DIRECTION ( 'NONE',  ( 0.9999836672264332815, -0.005715354789859956701, 0.000000000000000000 ) ) ;
#5932 = AXIS2_PLACEMENT_3D ( 'NONE', #5367, #2568, #200 ) ;
#5933 = AXIS2_PLACEMENT_3D ( 'NONE', #1422, #6701, #4901 ) ;
#5934 = CARTESIAN_POINT ( 'NONE',  ( 27.74658554044268399, 26.69867264686258679, -2.152344182241802795 ) ) ;
#5935 = CARTESIAN_POINT ( 'NONE',  ( 17.72531364449922719, -39.90520582355987500, -0.5137159595961888758 ) ) ;
#5936 = CARTESIAN_POINT ( 'NONE',  ( 5.465222000274489567, -57.03231251543625291, 0.2812537129946697800 ) ) ;
#5937 = VECTOR ( 'NONE', #2909, 1000.000000000000227 ) ;
#5938 = CARTESIAN_POINT ( 'NONE',  ( -5.207248779674009675, -62.02473276930714263, -2.515586951106906444 ) ) ;
#5939 = CARTESIAN_POINT ( 'NONE',  ( -14.70408710852078116, -35.66654345889202204, -3.000000000000036415 ) ) ;
#5940 = PLANE ( 'NONE',  #3721 ) ;
#5941 = ORIENTED_EDGE ( 'NONE', *, *, #6240, .T. ) ;
#5942 =( GEOMETRIC_REPRESENTATION_CONTEXT ( 3 ) GLOBAL_UNCERTAINTY_ASSIGNED_CONTEXT ( ( #3582 ) ) GLOBAL_UNIT_ASSIGNED_CONTEXT ( ( #2815, #2771, #78 ) ) REPRESENTATION_CONTEXT ( 'NONE', 'WORKASPACE' ) );
#5943 = VERTEX_POINT ( 'NONE', #6849 ) ;
#5944 = ORIENTED_EDGE ( 'NONE', *, *, #5846, .T. ) ;
#5945 = VERTEX_POINT ( 'NONE', #1694 ) ;
#5946 = AXIS2_PLACEMENT_3D ( 'NONE', #2833, #5752, #5674 ) ;
#5947 = CIRCLE ( 'NONE', #6068, 5.000000000000000000 ) ;
#5948 = CARTESIAN_POINT ( 'NONE',  ( -14.16308857960304302, 13.69107389482846315, 2.735642193797819921 ) ) ;
#5949 = CARTESIAN_POINT ( 'NONE',  ( 27.99155020439382469, -34.64269665048638558, -3.446982116472166490E-14 ) ) ;
#5950 = AXIS2_PLACEMENT_3D ( 'NONE', #2291, #600, #2888 ) ;
#5951 = CARTESIAN_POINT ( 'NONE',  ( 26.87031364676133194, -34.69479876584122024, -0.5000000000000345279 ) ) ;
#5952 = CARTESIAN_POINT ( 'NONE',  ( -5.253023064401910247, -61.29850624113154822, 1.730934016304810363 ) ) ;
#5953 = CIRCLE ( 'NONE', #6904, 0.9999999999999994449 ) ;
#5954 = ORIENTED_EDGE ( 'NONE', *, *, #7247, .F. ) ;
#5955 = AXIS2_PLACEMENT_3D ( 'NONE', #9, #5747, #686 ) ;
#5956 = ORIENTED_EDGE ( 'NONE', *, *, #1669, .F. ) ;
#5957 = VERTEX_POINT ( 'NONE', #567 ) ;
#5958 = AXIS2_PLACEMENT_3D ( 'NONE', #180, #6048, #6630 ) ;
#5959 = CARTESIAN_POINT ( 'NONE',  ( 0.000000000000000000, 0.000000000000000000, 0.000000000000000000 ) ) ;
#5960 = DIRECTION ( 'NONE',  ( 0.3144066910790611624, 0.9492883822130744331, 6.800116025829053242E-16 ) ) ;
#5961 = FACE_OUTER_BOUND ( 'NONE', #1046, .T. ) ;
#5962 = AXIS2_PLACEMENT_3D ( 'NONE', #3085, #5397, #7157 ) ;
#5963 = CARTESIAN_POINT ( 'NONE',  ( 35.41737116972092281, 6.499986109694644298, -1.499999999999993783 ) ) ;
#5964 = CYLINDRICAL_SURFACE ( 'NONE', #709, 3.250000000000000888 ) ;
#5965 = ORIENTED_EDGE ( 'NONE', *, *, #2721, .T. ) ;
#5966 = EDGE_CURVE ( 'NONE', #427, #5350, #2290, .T. ) ;
#5967 = DIRECTION ( 'NONE',  ( -0.9999836672264335036, 0.005715354789845041548, 0.000000000000000000 ) ) ;
#5968 = CARTESIAN_POINT ( 'NONE',  ( 1.218291106157554093, -66.23251464141941369, 3.139314518440670110 ) ) ;
#5969 = DIRECTION ( 'NONE',  ( -0.9147661038495522590, 0.4039838799357101107, 0.000000000000000000 ) ) ;
#5970 = DIRECTION ( 'NONE',  ( -0.9999836672264333925, 0.005715354789844970425, 0.000000000000000000 ) ) ;
#5971 = CARTESIAN_POINT ( 'NONE',  ( -0.9457358914118852988, -66.20977737079573444, -0.9048510307158501575 ) ) ;
#5972 = VERTEX_POINT ( 'NONE', #4339 ) ;
#5973 = DIRECTION ( 'NONE',  ( 0.4039838799357101107, 0.9147661038495522590, 4.900000000000001209E-14 ) ) ;
#5974 = ADVANCED_FACE ( 'NONE', ( #1287 ), #4143, .F. ) ;
#5975 = ADVANCED_FACE ( 'NONE', ( #6931 ), #539, .T. ) ;
#5976 = CARTESIAN_POINT ( 'NONE',  ( 9.311407240687648468, -51.41373841511902043, -1.002481404894999928 ) ) ;
#5977 = CARTESIAN_POINT ( 'NONE',  ( 17.91075855300138997, -40.39906292810271538, -0.2617559932753710794 ) ) ;
#5978 = FACE_OUTER_BOUND ( 'NONE', #6766, .T. ) ;
#5979 = CARTESIAN_POINT ( 'NONE',  ( -14.70408710852078116, -35.66654345889202204, -3.000000000000036415 ) ) ;
#5980 = CYLINDRICAL_SURFACE ( 'NONE', #1923, 5.000000000000001776 ) ;
#5981 = ORIENTED_EDGE ( 'NONE', *, *, #3696, .F. ) ;
#5982 = ORIENTED_EDGE ( 'NONE', *, *, #3705, .T. ) ;
#5983 = B_SPLINE_SURFACE_WITH_KNOTS ( 'NONE', 1, 3, ( 
 ( #7287, #2660, #2160, #931 ),
 ( #7214, #4321, #3818, #331 ) ),
 .UNSPECIFIED., .F., .F., .F.,
 ( 2, 2 ),
 ( 4, 4 ),
 ( 0.000000000000000000, 1.000000000000000000 ),
 ( 0.000000000000000000, 1.000000000000000000 ),
 .UNSPECIFIED. ) ;
#5984 = ADVANCED_FACE ( 'NONE', ( #3036 ), #4144, .T. ) ;
#5985 = DIRECTION ( 'NONE',  ( 5.715354789845004342E-18, 9.999836672264337477E-16, -1.000000000000000000 ) ) ;
#5986 = CARTESIAN_POINT ( 'NONE',  ( 35.53953323059130298, 5.908660390665234630, -1.055128867088183098 ) ) ;
#5987 = CARTESIAN_POINT ( 'NONE',  ( -5.207248779674009675, -62.02473276930714263, -2.515586951106906444 ) ) ;
#5988 = VERTEX_POINT ( 'NONE', #1249 ) ;
#5989 = ORIENTED_EDGE ( 'NONE', *, *, #3425, .T. ) ;
#5990 = ORIENTED_EDGE ( 'NONE', *, *, #5054, .F. ) ;
#5991 =( NAMED_UNIT ( * ) PLANE_ANGLE_UNIT ( ) SI_UNIT ( $, .RADIAN. ) );
#5992 = FACE_OUTER_BOUND ( 'NONE', #2500, .T. ) ;
#5993 = DIRECTION ( 'NONE',  ( 5.715354789845005112E-18, 9.999836672264339449E-16, -1.000000000000000000 ) ) ;
#5994 = CARTESIAN_POINT ( 'NONE',  ( 4.908910890503494606, -62.05094255708826978, -1.931865236676712838 ) ) ;
#5995 = CARTESIAN_POINT ( 'NONE',  ( -6.093803043304910183, -63.45548452497258296, 3.342215352752540447 ) ) ;
#5996 = EDGE_LOOP ( 'NONE', ( #2883, #4293, #3243, #67, #3454, #2727 ) ) ;
#5997 = VERTEX_POINT ( 'NONE', #5248 ) ;
#5998 = VERTEX_POINT ( 'NONE', #4066 ) ;
#5999 = CARTESIAN_POINT ( 'NONE',  ( 5.463696144088109996, -62.30361170774578028, -3.475027489484119769 ) ) ;
#6000 = CARTESIAN_POINT ( 'NONE',  ( -1.315849457849963988, -65.60036621133420454, 0.8401019477754300135 ) ) ;
#6001 = LINE ( 'NONE', #4376, #1907 ) ;
#6002 = CARTESIAN_POINT ( 'NONE',  ( 0.4753047092618455927, -54.67404102287693490, 0.1178634422923512670 ) ) ;
#6003 = EDGE_CURVE ( 'NONE', #1354, #5920, #1379, .T. ) ;
#6004 = ORIENTED_EDGE ( 'NONE', *, *, #6240, .F. ) ;
#6005 = DIRECTION ( 'NONE',  ( 0.5941197849118597940, 0.8043765792067080200, 8.077590468646243185E-16 ) ) ;
#6006 = DIRECTION ( 'NONE',  ( -0.9721221936972339606, -0.2344748185227520099, 0.000000000000000000 ) ) ;
#6007 = DIRECTION ( 'NONE',  ( 0.000000000000000000, -1.000000000000000000, -9.999836672264333533E-16 ) ) ;
#6008 = DIRECTION ( 'NONE',  ( -0.9147661038495488173, 0.4039838799357178822, 0.000000000000000000 ) ) ;
#6009 = CARTESIAN_POINT ( 'NONE',  ( 3.403992074353090036, -54.97443010399496899, 2.224669212202579960 ) ) ;
#6010 = CARTESIAN_POINT ( 'NONE',  ( -6.752862897928530117, -62.17267392066884213, 1.309913053057485177 ) ) ;
#6011 = EDGE_CURVE ( 'NONE', #7172, #3815, #3881, .T. ) ;
#6012 = DIRECTION ( 'NONE',  ( 1.000000000000000000, 0.000000000000000000, 0.000000000000000000 ) ) ;
#6013 = ADVANCED_FACE ( 'NONE', ( #5961 ), #6960, .T. ) ;
#6014 = VERTEX_POINT ( 'NONE', #1210 ) ;
#6015 = EDGE_LOOP ( 'NONE', ( #283, #1497 ) ) ;
#6016 = ORIENTED_EDGE ( 'NONE', *, *, #5377, .T. ) ;
#6017 = CARTESIAN_POINT ( 'NONE',  ( 69.23388681508718889, -35.19566595141640875, -3.469446951953614189E-14 ) ) ;
#6018 = AXIS2_PLACEMENT_3D ( 'NONE', #683, #3001, #1848 ) ;
#6019 = FACE_BOUND ( 'NONE', #5513, .T. ) ;
#6020 = CARTESIAN_POINT ( 'NONE',  ( 4.520351875826989385, -63.47384446676466752, 0.9302720625520102260 ) ) ;
#6021 = CARTESIAN_POINT ( 'NONE',  ( -2.400689227110559987, -66.32592643012861799, 1.119566937203962276 ) ) ;
#6022 = EDGE_CURVE ( 'NONE', #1124, #3341, #2937, .T. ) ;
#6023 = ORIENTED_EDGE ( 'NONE', *, *, #3219, .T. ) ;
#6024 = ORIENTED_EDGE ( 'NONE', *, *, #6641, .T. ) ;
#6025 = VERTEX_POINT ( 'NONE', #80 ) ;
#6026 = AXIS2_PLACEMENT_3D ( 'NONE', #4500, #2743, #6819 ) ;
#6027 = APPLICATION_CONTEXT ( 'automotive_design' ) ;
#6028 = APPLICATION_PROTOCOL_DEFINITION ( 'draft international standard', 'automotive_design', 1998, #3691 ) ;
#6029 = DIRECTION ( 'NONE',  ( -5.715354789860003484E-18, -9.999836672264337477E-16, 1.000000000000000000 ) ) ;
#6030 = CARTESIAN_POINT ( 'NONE',  ( -14.38395162568180652, 6.352317343304404673, 6.071532165918824830E-15 ) ) ;
#6031 = AXIS2_PLACEMENT_3D ( 'NONE', #3879, #2262, #6858 ) ;
#6032 = FACE_OUTER_BOUND ( 'NONE', #2316, .T. ) ;
#6033 = CARTESIAN_POINT ( 'NONE',  ( 6.131131505788760094, -57.13037711201883440, 2.282642250695309905 ) ) ;
#6034 = ORIENTED_EDGE ( 'NONE', *, *, #332, .T. ) ;
#6035 = EDGE_LOOP ( 'NONE', ( #3358, #3161, #4469, #3214 ) ) ;
#6036 = EDGE_LOOP ( 'NONE', ( #7300, #5537, #2801, #280, #2211, #1054, #1554, #174, #4186, #6698, #6281, #4903, #4241, #5613, #5395, #2501, #4055, #6842, #5191, #3296, #2046, #130, #1953, #4786, #778, #467, #3030, #2498, #2790, #328, #4652, #1891, #2373 ) ) ;
#6037 = CARTESIAN_POINT ( 'NONE',  ( -34.88460058024264043, 16.28046363954882736, -1.493845543551999944 ) ) ;
#6038 = CARTESIAN_POINT ( 'NONE',  ( -1.747150726250749964, -54.79256248330700174, -0.04158717877314997702 ) ) ;
#6039 = DIRECTION ( 'NONE',  ( -0.4328040977884316520, 0.5819352847797604200, 0.6884997728872834788 ) ) ;
#6040 = CARTESIAN_POINT ( 'NONE',  ( -95.86211798318534250, -102.0316339954322018, 3.999999999999897859 ) ) ;
#6041 = CARTESIAN_POINT ( 'NONE',  ( -5.772955398150772410, -60.86632288506189070, -0.4588952161651880246 ) ) ;
#6042 = VECTOR ( 'NONE', #7343, 1000.000000000000227 ) ;
#6043 = PRODUCT_DEFINITION_SHAPE ( 'NONE', 'NONE',  #7447 ) ;
#6044 = EDGE_LOOP ( 'NONE', ( #1002, #1197, #4182, #2626 ) ) ;
#6045 = LINE ( 'NONE', #1857, #5718 ) ;
#6046 = DIRECTION ( 'NONE',  ( -0.6713653717953970146, 0.7411265327553913096, 7.927884880413787584E-16 ) ) ;
#6047 = CARTESIAN_POINT ( 'NONE',  ( -14.63712380658832046, -35.33334692323139592, -3.626931576674818025 ) ) ;
#6048 = DIRECTION ( 'NONE',  ( 0.3144066910790611624, 0.9492883822130744331, 6.800116025829053242E-16 ) ) ;
#6049 = CARTESIAN_POINT ( 'NONE',  ( 1.414957918137925930, -67.26958221326191278, 2.900267041832249593 ) ) ;
#6050 = CYLINDRICAL_SURFACE ( 'NONE', #3128, 141.0000000000000284 ) ;
#6051 = CIRCLE ( 'NONE', #6998, 1.000000000000001110 ) ;
#6052 = CIRCLE ( 'NONE', #2303, 0.4999999999999991118 ) ;
#6053 = ORIENTED_EDGE ( 'NONE', *, *, #2071, .T. ) ;
#6054 = ORIENTED_EDGE ( 'NONE', *, *, #4263, .T. ) ;
#6055 = ORIENTED_EDGE ( 'NONE', *, *, #669, .F. ) ;
#6056 = LINE ( 'NONE', #1442, #5443 ) ;
#6057 = CIRCLE ( 'NONE', #3388, 0.5000000000000022204 ) ;
#6058 = AXIS2_PLACEMENT_3D ( 'NONE', #551, #2835, #5754 ) ;
#6059 = DIRECTION ( 'NONE',  ( 0.1845982795403122434, 0.9828140593167951078, 2.622080858921231671E-16 ) ) ;
#6060 = CARTESIAN_POINT ( 'NONE',  ( -4.816289696271150333, -61.50450503696147564, 2.285640538916479780 ) ) ;
#6061 = VECTOR ( 'NONE', #4444, 1000.000000000000000 ) ;
#6062 = DIRECTION ( 'NONE',  ( 0.000000000000000000, 0.000000000000000000, -1.000000000000000000 ) ) ;
#6063 = CARTESIAN_POINT ( 'NONE',  ( -2.881623215960232631, -54.84435829741126867, -0.2178263081526286560 ) ) ;
#6064 = VERTEX_POINT ( 'NONE', #5882 ) ;
#6065 = CONICAL_SURFACE ( 'NONE', #5095, 0.7499999999999865663, 1.029744258676651425 ) ;
#6066 = VERTEX_POINT ( 'NONE', #6994 ) ;
#6067 = ORIENTED_EDGE ( 'NONE', *, *, #2172, .T. ) ;
#6068 = AXIS2_PLACEMENT_3D ( 'NONE', #4089, #6394, #4552 ) ;
#6069 = ADVANCED_FACE ( 'NONE', ( #2336 ), #5810, .T. ) ;
#6070 = PRODUCT_CONTEXT ( 'NONE', #3312, 'mechanical' ) ;
#6071 = ADVANCED_FACE ( 'NONE', ( #2399 ), #5278, .T. ) ;
#6072 = DIRECTION ( 'NONE',  ( 0.9999836672264332815, -0.005715354789845002517, 0.000000000000000000 ) ) ;
#6073 = CIRCLE ( 'NONE', #164, 0.7500000000000000000 ) ;
#6074 = DIRECTION ( 'NONE',  ( -5.715354789845005112E-18, -9.999836672264339449E-16, 1.000000000000000000 ) ) ;
#6075 = LINE ( 'NONE', #7179, #529 ) ;
#6076 = CARTESIAN_POINT ( 'NONE',  ( 3.059030343303239974, -54.77303090793805040, 0.1039292770420399137 ) ) ;
#6077 = VERTEX_POINT ( 'NONE', #4676 ) ;
#6078 = VECTOR ( 'NONE', #4437, 1000.000000000000000 ) ;
#6079 = ORIENTED_EDGE ( 'NONE', *, *, #5246, .T. ) ;
#6080 = DIRECTION ( 'NONE',  ( 0.3128416502900970286, -0.9445788350777319931, 0.09950339776592319330 ) ) ;
#6081 = EDGE_CURVE ( 'NONE', #5703, #2927, #5111, .T. ) ;
#6082 = CARTESIAN_POINT ( 'NONE',  ( 5.216904734083789741, -62.90507476914316953, -1.366939949738901872 ) ) ;
#6083 = AXIS2_PLACEMENT_3D ( 'NONE', #7080, #3580, #3012 ) ;
#6084 = ORIENTED_EDGE ( 'NONE', *, *, #439, .F. ) ;
#6085 = DIRECTION ( 'NONE',  ( -0.9999836672264335036, 0.005715354789845008589, 0.000000000000000000 ) ) ;
#6086 = LINE ( 'NONE', #6667, #3965 ) ;
#6087 = AXIS2_PLACEMENT_3D ( 'NONE', #1503, #4249, #2590 ) ;
#6088 = ORIENTED_EDGE ( 'NONE', *, *, #1870, .T. ) ;
#6089 = DIRECTION ( 'NONE',  ( 0.9492899500389727629, 0.3144019573014849023, 0.000000000000000000 ) ) ;
#6090 = DIRECTION ( 'NONE',  ( 5.715354789860003484E-18, 9.999836672264337477E-16, -1.000000000000000000 ) ) ;
#6091 = DIRECTION ( 'NONE',  ( 0.000000000000000000, 0.000000000000000000, -1.000000000000000000 ) ) ;
#6092 = CARTESIAN_POINT ( 'NONE',  ( -17.04733905648494030, -8.234069079964157822, -3.000000000000009326 ) ) ;
#6093 = CARTESIAN_POINT ( 'NONE',  ( 6.775879105374429834, -62.07729961717699041, 0.4273099905340951299 ) ) ;
#6094 = CARTESIAN_POINT ( 'NONE',  ( 4.748085323256989732, -62.01668842780453872, -2.502390571778199568 ) ) ;
#6095 = ORIENTED_EDGE ( 'NONE', *, *, #6239, .T. ) ;
#6096 = LINE ( 'NONE', #7239, #1701 ) ;
#6097 = VERTEX_POINT ( 'NONE', #1838 ) ;
#6098 = DIRECTION ( 'NONE',  ( -0.9999836672264335036, 0.005715354789845041548, 0.000000000000000000 ) ) ;
#6099 = CARTESIAN_POINT ( 'NONE',  ( -7.547756740462723712, 12.24956608134465164, -2.993845543551527655 ) ) ;
#6100 = CARTESIAN_POINT ( 'NONE',  ( 2.734303695691099989, -65.14978033110251943, -1.014598242344157963 ) ) ;
#6101 = CARTESIAN_POINT ( 'NONE',  ( 14.29543924104632779, -35.83228874779774742, -3.556183125752454544E-14 ) ) ;
#6102 = CARTESIAN_POINT ( 'NONE',  ( 0.07924247749816264175, -66.69181187827942381, 3.086254127763143895 ) ) ;
#6103 = CARTESIAN_POINT ( 'NONE',  ( -5.466570931786790766, -63.95713299600960511, -2.842748680216657942 ) ) ;
#6104 = ORIENTED_EDGE ( 'NONE', *, *, #2956, .T. ) ;
#6105 = ADVANCED_FACE ( 'NONE', ( #3537 ), #1903, .T. ) ;
#6106 = ORIENTED_EDGE ( 'NONE', *, *, #1977, .T. ) ;
#6107 = EDGE_LOOP ( 'NONE', ( #1062, #1575, #478, #4015 ) ) ;
#6108 = DIRECTION ( 'NONE',  ( 0.000000000000000000, 0.000000000000000000, 1.000000000000000000 ) ) ;
#6109 = CARTESIAN_POINT ( 'NONE',  ( 94.42889356597736139, -103.2882618349535591, -1.027468802220174526E-13 ) ) ;
#6110 = CARTESIAN_POINT ( 'NONE',  ( -8.617355793880991044, 7.615193964809154004, -2.999999999999993339 ) ) ;
#6111 = DIRECTION ( 'NONE',  ( -0.9147661038495495944, 0.4039838799357160504, 3.987490689252424829E-16 ) ) ;
#6112 = CARTESIAN_POINT ( 'NONE',  ( 5.465222000274489567, -57.03231251543625291, 0.2812537129946697800 ) ) ;
#6113 = VERTEX_POINT ( 'NONE', #4710 ) ;
#6114 = EDGE_CURVE ( 'NONE', #6950, #6387, #6546, .T. ) ;
#6115 = EDGE_CURVE ( 'NONE', #2395, #5210, #7142, .T. ) ;
#6116 = DIRECTION ( 'NONE',  ( -0.9999836672264333925, 0.005715354789844388425, 0.000000000000000000 ) ) ;
#6117 = CARTESIAN_POINT ( 'NONE',  ( 5.267626090836840191, -63.86700364562991439, -1.442031773567929775 ) ) ;
#6118 = PLANE ( 'NONE',  #2396 ) ;
#6119 = CARTESIAN_POINT ( 'NONE',  ( -31.93002032970718318, 14.10110567601735632, -6.178731080732846159 ) ) ;
#6120 = EDGE_CURVE ( 'NONE', #354, #6909, #2932, .T. ) ;
#6121 = ORIENTED_EDGE ( 'NONE', *, *, #738, .F. ) ;
#6122 = CARTESIAN_POINT ( 'NONE',  ( -105.7473861751082040, -118.0666774205683822, -1.000000000000118794 ) ) ;
#6123 = LINE ( 'NONE', #868, #7129 ) ;
#6124 = CARTESIAN_POINT ( 'NONE',  ( -14.38395162568175145, 6.352317343304510366, -2.999999999999994671 ) ) ;
#6125 = CARTESIAN_POINT ( 'NONE',  ( 5.042816951933372316, 21.20642930254826553, -0.3999035282154982940 ) ) ;
#6126 = CARTESIAN_POINT ( 'NONE',  ( 2.082020516433249924, -53.40759131075155608, 1.446381639928540297 ) ) ;
#6127 = DIRECTION ( 'NONE',  ( -5.715354789860003484E-18, -9.999836672264337477E-16, 1.000000000000000000 ) ) ;
#6128 = ORIENTED_EDGE ( 'NONE', *, *, #4253, .T. ) ;
#6129 = CARTESIAN_POINT ( 'NONE',  ( 28.12455780688317475, -37.01391159201033076, -3.686287386450715076E-14 ) ) ;
#6130 = DIRECTION ( 'NONE',  ( -0.7811859829873639693, -0.4156127062761930113, 0.4658481924037536359 ) ) ;
#6131 = CARTESIAN_POINT ( 'NONE',  ( 12.34225220476766438, -34.27182074065601114, -3.426078865054194011E-14 ) ) ;
#6132 = CARTESIAN_POINT ( 'NONE',  ( 2.466033592522905327, -56.00841680802438560, -1.148886392136307943 ) ) ;
#6133 = CARTESIAN_POINT ( 'NONE',  ( 27.74785688037307096, -34.19481435285786830, 2.999999999999965805 ) ) ;
#6134 = CARTESIAN_POINT ( 'NONE',  ( -2.343653935680388933, -66.35127301696434188, 3.217364074058102652 ) ) ;
#6135 = VERTEX_POINT ( 'NONE', #3071 ) ;
#6136 = ORIENTED_EDGE ( 'NONE', *, *, #1988, .F. ) ;
#6137 = ORIENTED_EDGE ( 'NONE', *, *, #7022, .T. ) ;
#6138 = AXIS2_PLACEMENT_3D ( 'NONE', #6040, #941, #819 ) ;
#6139 = CARTESIAN_POINT ( 'NONE',  ( 1.714606436953501688E-17, 2.999951001679301835E-15, 0.000000000000000000 ) ) ;
#6140 = ADVANCED_FACE ( 'NONE', ( #1534 ), #5843, .T. ) ;
#6141 = DIRECTION ( 'NONE',  ( -0.9999836672264333925, 0.005715354789843017994, -1.984263399433601008E-30 ) ) ;
#6142 = LINE ( 'NONE', #7257, #4746 ) ;
#6143 = CARTESIAN_POINT ( 'NONE',  ( 3.318166867071405068, -54.31318850506334428, -0.01554017946999016950 ) ) ;
#6144 = ORIENTED_EDGE ( 'NONE', *, *, #2511, .T. ) ;
#6145 = CIRCLE ( 'NONE', #3959, 0.7500000000000002220 ) ;
#6146 = ORIENTED_EDGE ( 'NONE', *, *, #537, .F. ) ;
#6147 = CARTESIAN_POINT ( 'NONE',  ( 9.358334193258830425, -51.27205182843857045, -2.495037190209989930 ) ) ;
#6148 = DIRECTION ( 'NONE',  ( 5.715354789845005112E-18, 9.999836672264339449E-16, -1.000000000000000000 ) ) ;
#6149 = CARTESIAN_POINT ( 'NONE',  ( 4.841738599488129680, -63.57854475872899513, -1.322671891113719855 ) ) ;
#6150 = EDGE_CURVE ( 'NONE', #4378, #181, #7032, .T. ) ;
#6151 = CYLINDRICAL_SURFACE ( 'NONE', #4446, 6.299999999999999822 ) ;
#6152 = DIRECTION ( 'NONE',  ( 0.8039121061460987594, -0.3550279469270790633, 0.4771587602596087385 ) ) ;
#6153 = ORIENTED_EDGE ( 'NONE', *, *, #1539, .T. ) ;
#6154 = EDGE_CURVE ( 'NONE', #3586, #5920, #298, .T. ) ;
#6155 = DIRECTION ( 'NONE',  ( 5.715354789845005112E-18, 9.999836672264339449E-16, -1.000000000000000000 ) ) ;
#6156 = EDGE_CURVE ( 'NONE', #6227, #5128, #2098, .T. ) ;
#6157 = LINE ( 'NONE', #1997, #5583 ) ;
#6158 = FACE_OUTER_BOUND ( 'NONE', #3901, .T. ) ;
#6159 = CARTESIAN_POINT ( 'NONE',  ( -5.640317424943829927, -64.23513207997909547, 3.298613272382739936 ) ) ;
#6160 = DIRECTION ( 'NONE',  ( -5.715354789860003484E-18, -9.999836672264337477E-16, 1.000000000000000000 ) ) ;
#6161 = DIRECTION ( 'NONE',  ( -0.8688689365825387201, -0.4950421911735688463, -4.999999999999993486E-16 ) ) ;
#6162 = AXIS2_PLACEMENT_3D ( 'NONE', #4992, #4541, #7273 ) ;
#6163 = DIRECTION ( 'NONE',  ( 5.715354789845005112E-18, 9.999836672264339449E-16, -1.000000000000000000 ) ) ;
#6164 = EDGE_CURVE ( 'NONE', #4629, #1865, #6438, .T. ) ;
#6165 = CARTESIAN_POINT ( 'NONE',  ( -7.547756740462723712, 12.24956608134465164, -2.993845543551527655 ) ) ;
#6166 = AXIS2_PLACEMENT_3D ( 'NONE', #2689, #6748, #2082 ) ;
#6167 = CARTESIAN_POINT ( 'NONE',  ( -4.954937549494499827, -61.85628170826059602, 3.287035460711430268 ) ) ;
#6168 = CIRCLE ( 'NONE', #5932, 5.000000000000000000 ) ;
#6169 = DIRECTION ( 'NONE',  ( -5.715354789845005112E-18, -9.999836672264339449E-16, 1.000000000000000000 ) ) ;
#6170 = CARTESIAN_POINT ( 'NONE',  ( 27.11783474234811919, -35.12923323413248511, -1.000000000000035083 ) ) ;
#6171 = CARTESIAN_POINT ( 'NONE',  ( 5.248671903609490208, -63.99330799355751509, -3.505550301244489741 ) ) ;
#6172 = ORIENTED_EDGE ( 'NONE', *, *, #140, .F. ) ;
#6173 = VERTEX_POINT ( 'NONE', #6110 ) ;
#6174 = CYLINDRICAL_SURFACE ( 'NONE', #528, 3.299999999999999378 ) ;
#6175 = AXIS2_PLACEMENT_3D ( 'NONE', #2288, #3344, #3380 ) ;
#6176 = SURFACE_STYLE_FILL_AREA ( #4474 ) ;
#6177 = CARTESIAN_POINT ( 'NONE',  ( -19.94212619460463287, -40.63668738334721553, -3.000000000000041744 ) ) ;
#6178 = CARTESIAN_POINT ( 'NONE',  ( 43.89994888609457035, -93.87291691326068133, -9.367506770274758310E-14 ) ) ;
#6179 = CARTESIAN_POINT ( 'NONE',  ( 6.251545776960879763, -56.60079747432034480, -0.4089935619396500299 ) ) ;
#6180 = VECTOR ( 'NONE', #1307, 1000.000000000000000 ) ;
#6181 = TOROIDAL_SURFACE ( 'NONE', #1478, 147.0000000000000000, 1.000000000000000000 ) ;
#6182 = AXIS2_PLACEMENT_3D ( 'NONE', #844, #1532, #3855 ) ;
#6183 = DIRECTION ( 'NONE',  ( -0.8552446107963830313, -0.5182245224839744369, -5.231040848230092092E-16 ) ) ;
#6184 = CARTESIAN_POINT ( 'NONE',  ( -7.741417275248890562, 12.33509147838778830, 1.214306433183764966E-14 ) ) ;
#6185 = CARTESIAN_POINT ( 'NONE',  ( 5.676184037656430093, -63.13711808556965366, -1.485967351095627720 ) ) ;
#6186 = AXIS2_PLACEMENT_3D ( 'NONE', #1523, #581, #3474 ) ;
#6187 = AXIS2_PLACEMENT_3D ( 'NONE', #5279, #81, #2401 ) ;
#6188 = FACE_OUTER_BOUND ( 'NONE', #2100, .T. ) ;
#6189 = DIRECTION ( 'NONE',  ( 0.9999836672264335036, -0.005715354789845041548, 0.000000000000000000 ) ) ;
#6190 = ORIENTED_EDGE ( 'NONE', *, *, #1144, .F. ) ;
#6191 = EDGE_LOOP ( 'NONE', ( #1, #4682, #5445, #1854 ) ) ;
#6192 = EDGE_CURVE ( 'NONE', #6755, #216, #7141, .T. ) ;
#6193 = AXIS2_PLACEMENT_3D ( 'NONE', #3318, #5061, #2829 ) ;
#6194 = CYLINDRICAL_SURFACE ( 'NONE', #3749, 6.500000000000001776 ) ;
#6195 = CARTESIAN_POINT ( 'NONE',  ( 3.875821393968650330, 20.14928133654074927, 3.000000000000020428 ) ) ;
#6196 = CARTESIAN_POINT ( 'NONE',  ( 14.38741851828413942, 8.077882666870964457, -2.999999999999992895 ) ) ;
#6197 = TOROIDAL_SURFACE ( 'NONE', #1263, 1.500000000000000000, 1.000000000000000000 ) ;
#6198 = CARTESIAN_POINT ( 'NONE',  ( -6.487383171013251015, -57.01613561570176358, -1.117195879216653864 ) ) ;
#6199 = CYLINDRICAL_SURFACE ( 'NONE', #4861, 5.000000000000000000 ) ;
#6200 = EDGE_LOOP ( 'NONE', ( #890, #2079, #249, #1133 ) ) ;
#6201 = ADVANCED_FACE ( 'NONE', ( #256, #5422 ), #3747, .T. ) ;
#6202 = EDGE_CURVE ( 'NONE', #1143, #1865, #7178, .T. ) ;
#6203 = DIRECTION ( 'NONE',  ( 0.9999836672264335036, -0.005715354789845008589, 0.000000000000000000 ) ) ;
#6204 = CARTESIAN_POINT ( 'NONE',  ( -1.607783425601855054, -65.25734987882880489, 1.942476202525789342 ) ) ;
#6205 = CARTESIAN_POINT ( 'NONE',  ( 13.14859132361180194, 19.41219719266456423, 0.4060579846640096635 ) ) ;
#6206 = LINE ( 'NONE', #922, #2558 ) ;
#6207 = CARTESIAN_POINT ( 'NONE',  ( 4.447965418036755381, -62.61493371638615457, -2.739923498411994451 ) ) ;
#6208 = CARTESIAN_POINT ( 'NONE',  ( 27.63607196376285913, -34.25850433845761245, 3.508149587753143894 ) ) ;
#6209 = CARTESIAN_POINT ( 'NONE',  ( -40.82267254781529431, -94.88271315313488685, -9.511447951234663500E-14 ) ) ;
#6210 = VERTEX_POINT ( 'NONE', #848 ) ;
#6211 = EDGE_CURVE ( 'NONE', #1508, #4174, #1856, .T. ) ;
#6212 = ORIENTED_EDGE ( 'NONE', *, *, #5562, .F. ) ;
#6213 = ORIENTED_EDGE ( 'NONE', *, *, #5447, .T. ) ;
#6214 = SHAPE_DEFINITION_REPRESENTATION ( #3129, #5284 ) ;
#6215 = CARTESIAN_POINT ( 'NONE',  ( -31.91091272472834817, 16.82560631625344172, -2.993845543551523214 ) ) ;
#6216 = CARTESIAN_POINT ( 'NONE',  ( -17.21006346072928750, 13.86884027412869180, -2.230393353321906247 ) ) ;
#6217 = DIRECTION ( 'NONE',  ( 5.715354789845004342E-18, 9.999836672264337477E-16, -1.000000000000000000 ) ) ;
#6218 = DIRECTION ( 'NONE',  ( -5.715354789845005112E-18, -9.999836672264339449E-16, 1.000000000000000000 ) ) ;
#6219 = CARTESIAN_POINT ( 'NONE',  ( 3.357456528971034970, -66.96770758659590683, 2.241359037429140333 ) ) ;
#6220 = ORIENTED_EDGE ( 'NONE', *, *, #786, .F. ) ;
#6221 = EDGE_CURVE ( 'NONE', #4165, #5920, #4856, .T. ) ;
#6222 = CARTESIAN_POINT ( 'NONE',  ( 27.55235279947333993, -34.88166451341173513, 2.999999999999965361 ) ) ;
#6223 = CARTESIAN_POINT ( 'NONE',  ( -6.129265975028279634, -62.42766041111902098, -0.6909925287373350766 ) ) ;
#6224 = CARTESIAN_POINT ( 'NONE',  ( 39.97800414936823188, -95.26063634933134949, 2.999999999999904965 ) ) ;
#6225 = CARTESIAN_POINT ( 'NONE',  ( -22.27644891976294161, 9.837844043328894728, -2.993845543551520105 ) ) ;
#6226 = DIRECTION ( 'NONE',  ( -5.715354789860003484E-18, -9.999836672264337477E-16, 1.000000000000000000 ) ) ;
#6227 = VERTEX_POINT ( 'NONE', #222 ) ;
#6228 = DIRECTION ( 'NONE',  ( -0.9999836672264335036, 0.005715354789845008589, 0.000000000000000000 ) ) ;
#6229 = CARTESIAN_POINT ( 'NONE',  ( -5.480856739662490540, -62.25220485324549458, 1.560007870815685260 ) ) ;
#6230 = EDGE_CURVE ( 'NONE', #2342, #6356, #2817, .T. ) ;
#6231 = DIRECTION ( 'NONE',  ( -0.9999836672264333925, 0.005715354789844984303, 0.000000000000000000 ) ) ;
#6232 = CARTESIAN_POINT ( 'NONE',  ( -7.175161506198990402, -58.91160695923000645, -1.204451995733903935 ) ) ;
#6233 = CARTESIAN_POINT ( 'NONE',  ( 27.11783474234813340, -35.12923323413248511, 3.999999999999965361 ) ) ;
#6234 = ORIENTED_EDGE ( 'NONE', *, *, #6393, .T. ) ;
#6235 = DIRECTION ( 'NONE',  ( 5.715354789845005112E-18, 9.999836672264339449E-16, -1.000000000000000000 ) ) ;
#6236 = CARTESIAN_POINT ( 'NONE',  ( 1.460134286533229853, -55.58368472982129305, 0.8822880931559249351 ) ) ;
#6237 = DIRECTION ( 'NONE',  ( 0.1860016876085203441, -0.1636620475539279917, 0.9688230521603200529 ) ) ;
#6238 = CARTESIAN_POINT ( 'NONE',  ( 15.26844188666829893, -16.88471001685938333, -1.691355389077386917E-14 ) ) ;
#6239 = EDGE_CURVE ( 'NONE', #7415, #1143, #3542, .T. ) ;
#6240 = EDGE_CURVE ( 'NONE', #5840, #3712, #1267, .T. ) ;
#6241 = CARTESIAN_POINT ( 'NONE',  ( 18.11147093304812827, -39.68519087974932802, -0.2612916689653262403 ) ) ;
#6242 = CARTESIAN_POINT ( 'NONE',  ( 0.002312830554035623463, -66.69201937025515292, -1.109451928479881833 ) ) ;
#6243 = ORIENTED_EDGE ( 'NONE', *, *, #5599, .F. ) ;
#6244 = ORIENTED_EDGE ( 'NONE', *, *, #3052, .T. ) ;
#6245 = CARTESIAN_POINT ( 'NONE',  ( 18.38437121370851202, -39.52970465251538457, 3.499999999999965805 ) ) ;
#6246 = ORIENTED_EDGE ( 'NONE', *, *, #2365, .F. ) ;
#6247 = CARTESIAN_POINT ( 'NONE',  ( 41.70778007397900211, -94.98992620957551480, 2.999999999999905409 ) ) ;
#6248 = EDGE_CURVE ( 'NONE', #5350, #1170, #333, .T. ) ;
#6249 = ADVANCED_FACE ( 'NONE', ( #4967 ), #5467, .T. ) ;
#6250 = CYLINDRICAL_SURFACE ( 'NONE', #1843, 1.000000000000000888 ) ;
#6251 = CARTESIAN_POINT ( 'NONE',  ( 18.74668230531430169, -39.89873697698325117, 3.999999999999960032 ) ) ;
#6252 = CARTESIAN_POINT ( 'NONE',  ( 7.059059989562619819, -58.43975188330606585, -0.3221438859163246460 ) ) ;
#6253 = TOROIDAL_SURFACE ( 'NONE', #6018, 1.500000000000000000, 1.000000000000000000 ) ;
#6254 = FACE_OUTER_BOUND ( 'NONE', #6634, .T. ) ;
#6255 = DIRECTION ( 'NONE',  ( 0.2164621326156030423, -0.07169280077033016174, 0.9736551173085935540 ) ) ;
#6256 = CARTESIAN_POINT ( 'NONE',  ( -16.51707533432788111, -40.85914143033993895, -3.000000000000041744 ) ) ;
#6257 = EDGE_CURVE ( 'NONE', #3446, #5680, #6783, .T. ) ;
#6258 = LINE ( 'NONE', #2027, #5480 ) ;
#6259 = AXIS2_PLACEMENT_3D ( 'NONE', #3956, #3353, #3316 ) ;
#6260 = LINE ( 'NONE', #1621, #5898 ) ;
#6261 = DIRECTION ( 'NONE',  ( 5.715354789860003484E-18, 9.999836672264337477E-16, -1.000000000000000000 ) ) ;
#6262 = ORIENTED_EDGE ( 'NONE', *, *, #343, .F. ) ;
#6263 = CIRCLE ( 'NONE', #7212, 147.0000000000000284 ) ;
#6264 = DIRECTION ( 'NONE',  ( -5.715354789845005112E-18, -9.999836672264339449E-16, 1.000000000000000000 ) ) ;
#6265 = CARTESIAN_POINT ( 'NONE',  ( 27.55235279947335414, -34.88166451341171381, -3.471129529363089628E-14 ) ) ;
#6266 = CARTESIAN_POINT ( 'NONE',  ( -109.1076725891878567, -112.1689003517234227, 2.999999999999887201 ) ) ;
#6267 = MECHANICAL_DESIGN_GEOMETRIC_PRESENTATION_REPRESENTATION (  '', ( #1913 ), #5666 ) ;
#6268 = CARTESIAN_POINT ( 'NONE',  ( 1.647105754412080181, -53.29316706828264216, -0.6741030570719998005 ) ) ;
#6269 = PLANE ( 'NONE',  #3287 ) ;
#6270 = ORIENTED_EDGE ( 'NONE', *, *, #1743, .F. ) ;
#6271 = DIRECTION ( 'NONE',  ( -0.4039838799357114985, -0.9147661038495515928, -8.673617379884191272E-16 ) ) ;
#6272 = ADVANCED_FACE ( 'NONE', ( #3859 ), #5039, .F. ) ;
#6273 = CARTESIAN_POINT ( 'NONE',  ( -5.121204309455420045, -61.36711808260334067, 3.320501707867800523 ) ) ;
#6274 = VECTOR ( 'NONE', #1861, 1000.000000000000000 ) ;
#6275 = LINE ( 'NONE', #13, #5831 ) ;
#6276 = DIRECTION ( 'NONE',  ( -0.8688689365825387201, -0.4950421911735688463, -4.999999999999993486E-16 ) ) ;
#6277 = CARTESIAN_POINT ( 'NONE',  ( 2.751515497641074948, -64.99867735210931130, 0.5749532485596650089 ) ) ;
#6278 = CARTESIAN_POINT ( 'NONE',  ( 26.92746976600782816, -34.66223379623596657, 3.499999971184567293 ) ) ;
#6279 = DIRECTION ( 'NONE',  ( -0.9793199139485100346, -0.2023178344681531293, -1.787644449902631965E-16 ) ) ;
#6280 = AXIS2_PLACEMENT_3D ( 'NONE', #6565, #1405, #4882 ) ;
#6281 = ORIENTED_EDGE ( 'NONE', *, *, #3963, .T. ) ;
#6282 = ORIENTED_EDGE ( 'NONE', *, *, #1400, .T. ) ;
#6283 = ORIENTED_EDGE ( 'NONE', *, *, #27, .F. ) ;
#6284 = CARTESIAN_POINT ( 'NONE',  ( -14.16308857960304302, 13.69107389482846315, 2.735642193797819921 ) ) ;
#6285 = LINE ( 'NONE', #2843, #4367 ) ;
#6286 = DIRECTION ( 'NONE',  ( -5.715354789860003484E-18, -9.999836672264337477E-16, 1.000000000000000000 ) ) ;
#6287 = DIRECTION ( 'NONE',  ( 5.715354789845084461E-18, 9.999836672264339449E-16, -1.000000000000000000 ) ) ;
#6288 = CARTESIAN_POINT ( 'NONE',  ( -6.429839020462739363, -63.58404662519255623, 2.770540757372710328 ) ) ;
#6289 = ORIENTED_EDGE ( 'NONE', *, *, #6599, .T. ) ;
#6290 = EDGE_LOOP ( 'NONE', ( #5757, #139, #3109, #2223 ) ) ;
#6291 = VECTOR ( 'NONE', #717, 1000.000000000000000 ) ;
#6292 = ADVANCED_FACE ( 'NONE', ( #2208 ), #1257, .F. ) ;
#6293 = LINE ( 'NONE', #5011, #383 ) ;
#6294 = EDGE_CURVE ( 'NONE', #4841, #3587, #6880, .T. ) ;
#6295 = MECHANICAL_DESIGN_GEOMETRIC_PRESENTATION_REPRESENTATION (  '', ( #5594 ), #4260 ) ;
#6296 = CARTESIAN_POINT ( 'NONE',  ( 10.77958151816464216, 24.37277465456891079, 3.306154456448493484 ) ) ;
#6297 = CARTESIAN_POINT ( 'NONE',  ( 26.82878048574519525, 24.30342645899339971, 2.428612866367529932E-14 ) ) ;
#6298 = CARTESIAN_POINT ( 'NONE',  ( -3.749938752099124972, 0.02143258046197846906, -3.000000000000000888 ) ) ;
#6299 = AXIS2_PLACEMENT_3D ( 'NONE', #2478, #3598, #3143 ) ;
#6300 = FACE_OUTER_BOUND ( 'NONE', #1223, .T. ) ;
#6301 = CARTESIAN_POINT ( 'NONE',  ( 18.04796579205319063, 16.34913706177017545, 0.006154456448481410852 ) ) ;
#6302 = VECTOR ( 'NONE', #6148, 1000.000000000000000 ) ;
#6303 = ORIENTED_EDGE ( 'NONE', *, *, #3696, .T. ) ;
#6304 = VECTOR ( 'NONE', #1112, 1000.000000000000000 ) ;
#6305 = AXIS2_PLACEMENT_3D ( 'NONE', #2122, #894, #2659 ) ;
#6306 = AXIS2_PLACEMENT_3D ( 'NONE', #2282, #144, #1875 ) ;
#6307 = CARTESIAN_POINT ( 'NONE',  ( 18.38526242690743118, -39.52919687957394501, 4.002803558047675736 ) ) ;
#6308 = FACE_OUTER_BOUND ( 'NONE', #1863, .T. ) ;
#6309 = AXIS2_PLACEMENT_3D ( 'NONE', #4655, #4, #4611 ) ;
#6310 = CARTESIAN_POINT ( 'NONE',  ( -45.28625779897078729, -94.36209361619114588, -3.000000000000095479 ) ) ;
#6311 = CARTESIAN_POINT ( 'NONE',  ( 6.738276468386390050, -62.65933952543014129, -2.221138621355481568 ) ) ;
#6312 = ORIENTED_EDGE ( 'NONE', *, *, #7361, .T. ) ;
#6313 = DIRECTION ( 'NONE',  ( -0.9147661038495522590, 0.4039838799357101107, 0.000000000000000000 ) ) ;
#6314 = CARTESIAN_POINT ( 'NONE',  ( 17.91074121684488674, -40.39907330555904963, -0.2616656984610406522 ) ) ;
#6315 = VECTOR ( 'NONE', #7193, 1000.000000000000000 ) ;
#6316 = FACE_OUTER_BOUND ( 'NONE', #6200, .T. ) ;
#6317 = CARTESIAN_POINT ( 'NONE',  ( -5.163597282883630513, -63.01551968439245144, 3.580859834736030312 ) ) ;
#6318 = CARTESIAN_POINT ( 'NONE',  ( 27.11783474234813340, -35.12923323413248511, 3.999999999999965361 ) ) ;
#6319 = CARTESIAN_POINT ( 'NONE',  ( 0.000000000000000000, 0.000000000000000000, -17.67054229618195293 ) ) ;
#6320 = ORIENTED_EDGE ( 'NONE', *, *, #1650, .F. ) ;
#6321 = ORIENTED_EDGE ( 'NONE', *, *, #339, .T. ) ;
#6322 = VERTEX_POINT ( 'NONE', #7323 ) ;
#6323 = VERTEX_POINT ( 'NONE', #3903 ) ;
#6324 = CARTESIAN_POINT ( 'NONE',  ( 43.95483829995806957, -94.87490738911687060, -9.454242944073598665E-14 ) ) ;
#6325 = ORIENTED_EDGE ( 'NONE', *, *, #1314, .T. ) ;
#6326 = CARTESIAN_POINT ( 'NONE',  ( -9.311346830843410416, -51.41373841511902043, 3.533728595105000370 ) ) ;
#6327 = CARTESIAN_POINT ( 'NONE',  ( -6.026503769217380402, -56.70691413961192495, -0.01483612153302480557 ) ) ;
#6328 = CARTESIAN_POINT ( 'NONE',  ( -5.788105944719140084, -64.22553544194731501, 1.709038299673605321 ) ) ;
#6329 = ADVANCED_FACE ( 'NONE', ( #4555 ), #2163, .T. ) ;
#6330 = ORIENTED_EDGE ( 'NONE', *, *, #6768, .T. ) ;
#6331 = ORIENTED_EDGE ( 'NONE', *, *, #451, .T. ) ;
#6332 = CARTESIAN_POINT ( 'NONE',  ( 27.34642260356996246, -35.00195026692180988, -0.9740222605457664606 ) ) ;
#6333 = DIRECTION ( 'NONE',  ( 7.436638807346758235E-18, 1.301147106321757529E-15, -1.000000000000000000 ) ) ;
#6334 = CARTESIAN_POINT ( 'NONE',  ( -33.11453295935376673, 14.62421645367269463, 1.431146867680865853E-14 ) ) ;
#6335 = CARTESIAN_POINT ( 'NONE',  ( 9.998427761233271482, -32.39925913208585939, -3.252606517456513302E-14 ) ) ;
#6336 = CARTESIAN_POINT ( 'NONE',  ( 27.99155020439384955, -34.64269665048637137, 3.132057286715485667 ) ) ;
#6337 = ADVANCED_FACE ( 'NONE', ( #1614 ), #6250, .T. ) ;
#6338 =( NAMED_UNIT ( * ) SI_UNIT ( $, .STERADIAN. ) SOLID_ANGLE_UNIT ( ) );
#6339 = VERTEX_POINT ( 'NONE', #6177 ) ;
#6340 = ORIENTED_EDGE ( 'NONE', *, *, #542, .F. ) ;
#6341 = CARTESIAN_POINT ( 'NONE',  ( 18.07587756468298679, -39.70547036992888223, 3.131697286032659733 ) ) ;
#6342 = DIRECTION ( 'NONE',  ( -7.159176919053500386E-18, -9.973300763855708376E-16, 1.000000000000000000 ) ) ;
#6343 = ADVANCED_FACE ( 'NONE', ( #2124 ), #3940, .F. ) ;
#6344 = CARTESIAN_POINT ( 'NONE',  ( -45.28625779897078729, -94.36209361619114588, -3.000000000000095479 ) ) ;
#6345 = CARTESIAN_POINT ( 'NONE',  ( 6.291895255447879975, -62.07086823355334104, -1.517278733858541839 ) ) ;
#6346 = DIRECTION ( 'NONE',  ( -5.715354789845005112E-18, -9.999836672264339449E-16, 1.000000000000000000 ) ) ;
#6347 = VERTEX_POINT ( 'NONE', #5649 ) ;
#6348 = DIRECTION ( 'NONE',  ( 0.9999836672264335036, -0.005715354789845041548, 0.000000000000000000 ) ) ;
#6349 =( NAMED_UNIT ( * ) SI_UNIT ( $, .STERADIAN. ) SOLID_ANGLE_UNIT ( ) );
#6350 = FACE_OUTER_BOUND ( 'NONE', #665, .T. ) ;
#6351 = CARTESIAN_POINT ( 'NONE',  ( -1.095027572700850049, -66.25608112803911354, -0.9253912358714898589 ) ) ;
#6352 = CARTESIAN_POINT ( 'NONE',  ( 27.13760594192228481, -34.54250771490235650, 3.399562066569207897 ) ) ;
#6353 = CARTESIAN_POINT ( 'NONE',  ( 27.68174825049008803, -37.24611774345110859, 2.999999999999962697 ) ) ;
#6354 = EDGE_LOOP ( 'NONE', ( #342, #1964, #1623, #6243 ) ) ;
#6355 = VERTEX_POINT ( 'NONE', #1571 ) ;
#6356 = VERTEX_POINT ( 'NONE', #2808 ) ;
#6357 = ORIENTED_EDGE ( 'NONE', *, *, #2035, .F. ) ;
#6358 = CARTESIAN_POINT ( 'NONE',  ( -15.02360761328580097, -37.34705832593169816, 1.026284428608169819 ) ) ;
#6359 = CARTESIAN_POINT ( 'NONE',  ( 26.67188031194815068, 24.16129507000589172, 0.006154456448489217107 ) ) ;
#6360 = CARTESIAN_POINT ( 'NONE',  ( 6.364381519408680354, -59.13673167413750775, 0.4262454961123699482 ) ) ;
#6361 = DIRECTION ( 'NONE',  ( -5.715354789845005112E-18, -9.999836672264339449E-16, 1.000000000000000000 ) ) ;
#6362 = CARTESIAN_POINT ( 'NONE',  ( -2.818432829560444830, -65.09919931551695527, -0.6601304211325950133 ) ) ;
#6363 = ORIENTED_EDGE ( 'NONE', *, *, #5054, .T. ) ;
#6364 = ADVANCED_FACE ( 'NONE', ( #484, #4025, #966 ), #3256, .T. ) ;
#6365 = DIRECTION ( 'NONE',  ( 0.9999836672264333925, -0.005715354789844388425, 0.000000000000000000 ) ) ;
#6366 = CARTESIAN_POINT ( 'NONE',  ( 43.45632180942044442, -94.90042465344848210, 2.999999999999905409 ) ) ;
#6367 = CARTESIAN_POINT ( 'NONE',  ( -32.92087242456759100, 14.53869105662955796, -2.993845543551514776 ) ) ;
#6368 = CARTESIAN_POINT ( 'NONE',  ( -32.93157973858376408, 14.54341967768581867, -2.999999999999986677 ) ) ;
#6369 = CARTESIAN_POINT ( 'NONE',  ( 5.661113010068490325, -57.37064013373739613, 2.401523511004880262 ) ) ;
#6370 = CARTESIAN_POINT ( 'NONE',  ( 22.93267937958135860, 20.84152453766674284, -1.493845543551514332 ) ) ;
#6371 = ORIENTED_EDGE ( 'NONE', *, *, #4909, .F. ) ;
#6372 = DIRECTION ( 'NONE',  ( 2.290931512739800066E-16, 1.403768413105889815E-16, 1.000000000000000000 ) ) ;
#6373 = CARTESIAN_POINT ( 'NONE',  ( 3.749938752099124972, -0.02143258046191875987, 3.000000000000000000 ) ) ;
#6374 = CARTESIAN_POINT ( 'NONE',  ( 4.121185724914560033, -64.58760431682401304, 0.8784256758975720336 ) ) ;
#6375 = DIRECTION ( 'NONE',  ( 5.715354789860003484E-18, 9.999836672264337477E-16, -1.000000000000000000 ) ) ;
#6376 = CIRCLE ( 'NONE', #1805, 5.000000000000000000 ) ;
#6377 = ORIENTED_EDGE ( 'NONE', *, *, #4995, .T. ) ;
#6378 = DIRECTION ( 'NONE',  ( -0.9147661038495529251, 0.4039838799357087229, 3.942553354492743531E-16 ) ) ;
#6379 = EDGE_CURVE ( 'NONE', #1750, #2698, #6535, .T. ) ;
#6380 = ADVANCED_FACE ( 'NONE', ( #452 ), #4475, .F. ) ;
#6381 =( LENGTH_UNIT ( ) NAMED_UNIT ( * ) SI_UNIT ( .MILLI., .METRE. ) );
#6382 = AXIS2_PLACEMENT_3D ( 'NONE', #3194, #3869, #6189 ) ;
#6383 = DIRECTION ( 'NONE',  ( -0.9999836672264333925, 0.005715354789844388425, 0.000000000000000000 ) ) ;
#6384 = CARTESIAN_POINT ( 'NONE',  ( 5.677676720488819662, -58.78440004686129328, 0.4885712913175552785 ) ) ;
#6385 = CARTESIAN_POINT ( 'NONE',  ( -3.498019654714389581, -55.03494779767484602, -0.2490962732230048438 ) ) ;
#6386 = DIRECTION ( 'NONE',  ( -5.715354789860003484E-18, -9.999836672264337477E-16, 1.000000000000000000 ) ) ;
#6387 = VERTEX_POINT ( 'NONE', #1126 ) ;
#6388 = ORIENTED_EDGE ( 'NONE', *, *, #2674, .F. ) ;
#6389 = ORIENTED_EDGE ( 'NONE', *, *, #4849, .T. ) ;
#6390 = ORIENTED_EDGE ( 'NONE', *, *, #1145, .F. ) ;
#6391 = VECTOR ( 'NONE', #1740, 1000.000000000000114 ) ;
#6392 = PRODUCT ( 'Vinyl Handle Grips', 'Vinyl Handle Grips', '', ( #1721 ) ) ;
#6393 = EDGE_CURVE ( 'NONE', #961, #4283, #6761, .T. ) ;
#6394 = DIRECTION ( 'NONE',  ( 5.715354789845005112E-18, 9.999836672264339449E-16, -1.000000000000000000 ) ) ;
#6395 = DIRECTION ( 'NONE',  ( -3.872980802086269402E-16, 2.250611045722691657E-16, -1.000000000000000000 ) ) ;
#6396 = CARTESIAN_POINT ( 'NONE',  ( -6.338727533122220592, -59.01378846946391832, -2.577673957235475211 ) ) ;
#6397 = DIRECTION ( 'NONE',  ( 0.9999836672264332815, -0.005715354789845002517, 0.000000000000000000 ) ) ;
#6398 = VERTEX_POINT ( 'NONE', #6804 ) ;
#6399 = AXIS2_PLACEMENT_3D ( 'NONE', #1155, #7425, #2381 ) ;
#6400 = CARTESIAN_POINT ( 'NONE',  ( -28.22553731214382111, -35.79092421365019305, -3.001000000000037193 ) ) ;
#6401 = DIRECTION ( 'NONE',  ( -0.9492899500389727629, -0.3144019573014849023, 0.000000000000000000 ) ) ;
#6402 = B_SPLINE_CURVE_WITH_KNOTS ( 'NONE', 3,
 ( #4604, #6336, #6812, #1021, #1059, #1655, #2889, #5773 ),
 .UNSPECIFIED., .F., .F.,
 ( 4, 2, 2, 4 ),
 ( 4.336808689942017736E-18, 0.0003905499302250284256, 0.0007810998604500525144, 0.001562199720900107631 ),
 .UNSPECIFIED. ) ;
#6403 = APPLICATION_CONTEXT ( 'automotive_design' ) ;
#6404 = LINE ( 'NONE', #6442, #5473 ) ;
#6405 = CARTESIAN_POINT ( 'NONE',  ( -1.592557218785495055, -66.68601476236933934, 1.076257986235874764 ) ) ;
#6406 = CARTESIAN_POINT ( 'NONE',  ( 43.45632180942044442, -94.90042465344848210, -9.454242944073598665E-14 ) ) ;
#6407 = AXIS2_PLACEMENT_3D ( 'NONE', #1877, #7170, #3040 ) ;
#6408 = AXIS2_PLACEMENT_3D ( 'NONE', #572, #6816, #6228 ) ;
#6409 = CARTESIAN_POINT ( 'NONE',  ( -2.954381708604445045, -64.87272166844897470, 3.050067095118260241 ) ) ;
#6410 = CIRCLE ( 'NONE', #398, 2.500000000000000000 ) ;
#6411 = CARTESIAN_POINT ( 'NONE',  ( -3.888488774788935842, -0.9378992740910081505, -17.67054229618195293 ) ) ;
#6412 = STYLED_ITEM ( 'NONE', ( #6847 ), #7333 ) ;
#6413 = CARTESIAN_POINT ( 'NONE',  ( -95.86211798318534250, -102.0316339954322018, 2.999999999999897859 ) ) ;
#6414 = CARTESIAN_POINT ( 'NONE',  ( 14.63763862841553376, 20.11382921380832656, 0.006154456448485313980 ) ) ;
#6415 = CARTESIAN_POINT ( 'NONE',  ( 6.364381519408680354, -59.13673167413750775, 0.4262454961123699482 ) ) ;
#6416 = ADVANCED_FACE ( 'NONE', ( #3416 ), #1086, .F. ) ;
#6417 = DIRECTION ( 'NONE',  ( 0.2223157560262043198, -0.6712493609847984821, 0.7071067811865453523 ) ) ;
#6418 = AXIS2_PLACEMENT_3D ( 'NONE', #2391, #4701, #6987 ) ;
#6419 = CIRCLE ( 'NONE', #5826, 2.500000000000000000 ) ;
#6420 = ORIENTED_EDGE ( 'NONE', *, *, #802, .T. ) ;
#6421 = CARTESIAN_POINT ( 'NONE',  ( -14.70408710852078116, -35.66654345889202204, -3.575000000000001175E-14 ) ) ;
#6422 = CARTESIAN_POINT ( 'NONE',  ( 17.61082880304171994, -39.97043410412674547, -3.981171391688891273E-14 ) ) ;
#6423 = CARTESIAN_POINT ( 'NONE',  ( 1.218291106157554093, -66.23251464141941369, 3.139314518440670110 ) ) ;
#6424 = PRESENTATION_LAYER_ASSIGNMENT (  '', '', ( #5594 ) ) ;
#6425 = CARTESIAN_POINT ( 'NONE',  ( 1.402950248545461909, -54.15620739517822813, 0.01614447287717020105 ) ) ;
#6426 = EDGE_CURVE ( 'NONE', #3534, #3922, #2844, .T. ) ;
#6427 = DIRECTION ( 'NONE',  ( -0.2023178344681547114, 0.9793199139485095905, 8.673617379884032514E-16 ) ) ;
#6428 = EDGE_CURVE ( 'NONE', #7272, #1033, #408, .T. ) ;
#6429 = ORIENTED_EDGE ( 'NONE', *, *, #1351, .F. ) ;
#6430 = ORIENTED_EDGE ( 'NONE', *, *, #6968, .F. ) ;
#6431 = AXIS2_PLACEMENT_3D ( 'NONE', #5656, #2819, #6626 ) ;
#6432 = CARTESIAN_POINT ( 'NONE',  ( -15.80406914246985650, -35.66025656862317561, -3.000000000000036415 ) ) ;
#6433 = CARTESIAN_POINT ( 'NONE',  ( -33.94153943842304955, 12.25650441806195445, 1.206231629534596424E-14 ) ) ;
#6434 = CARTESIAN_POINT ( 'NONE',  ( -6.176129832103540274, -61.75772637036916279, 1.476179264717100370 ) ) ;
#6435 = CARTESIAN_POINT ( 'NONE',  ( 27.99155020466450949, -34.64269665098379392, -0.1315720824427292768 ) ) ;
#6436 = ORIENTED_EDGE ( 'NONE', *, *, #4849, .F. ) ;
#6437 = EDGE_CURVE ( 'NONE', #5945, #5232, #4648, .T. ) ;
#6438 = CIRCLE ( 'NONE', #6087, 4.000000000000000000 ) ;
#6439 = EDGE_LOOP ( 'NONE', ( #2246, #1117, #1004, #2802 ) ) ;
#6440 = CYLINDRICAL_SURFACE ( 'NONE', #4976, 2.500000000000000000 ) ;
#6441 = CARTESIAN_POINT ( 'NONE',  ( 1.714606436953501688E-17, 2.999951001679301835E-15, 0.000000000000000000 ) ) ;
#6442 = CARTESIAN_POINT ( 'NONE',  ( 11.49981217310398485, -0.06572658008321453915, 0.000000000000000000 ) ) ;
#6443 = CARTESIAN_POINT ( 'NONE',  ( 41.70778007397900211, -94.98992620957551480, 3.999999999999905409 ) ) ;
#6444 = CARTESIAN_POINT ( 'NONE',  ( 1.990789772983897477, -66.41826147249288681, 0.8834450765732816402 ) ) ;
#6445 = CARTESIAN_POINT ( 'NONE',  ( 5.257784700090706309, -62.23303559029498899, -3.424757160461740835 ) ) ;
#6446 = CARTESIAN_POINT ( 'NONE',  ( -27.72086689141922022, 13.93665911791816470, -1.493845543551521216 ) ) ;
#6447 = CARTESIAN_POINT ( 'NONE',  ( -1.721951098409294945, -66.71030961465282871, -0.9872116442447198548 ) ) ;
#6448 = ORIENTED_EDGE ( 'NONE', *, *, #5741, .F. ) ;
#6449 = DIRECTION ( 'NONE',  ( 0.3128463504745285229, 0.9445772445362839997, 0.09950371902099811039 ) ) ;
#6450 = EDGE_CURVE ( 'NONE', #5997, #6064, #875, .T. ) ;
#6451 = DIRECTION ( 'NONE',  ( 0.2164621326156030423, -0.07169280077033016174, 0.9736551173085935540 ) ) ;
#6452 = CARTESIAN_POINT ( 'NONE',  ( 18.28020160475467293, -39.58905578051523122, -0.4368566607114584555 ) ) ;
#6453 = CARTESIAN_POINT ( 'NONE',  ( -1.397697773942189858, -54.69607029038206747, 2.078897745975250455 ) ) ;
#6454 = CARTESIAN_POINT ( 'NONE',  ( 5.676184037656430093, -63.13711808556965366, -1.485967351095627720 ) ) ;
#6455 = LINE ( 'NONE', #2312, #967 ) ;
#6456 = ORIENTED_EDGE ( 'NONE', *, *, #2215, .T. ) ;
#6457 = EDGE_LOOP ( 'NONE', ( #7200, #6834, #3329, #2350 ) ) ;
#6458 = ORIENTED_EDGE ( 'NONE', *, *, #3293, .T. ) ;
#6459 = EDGE_CURVE ( 'NONE', #3446, #6558, #6404, .T. ) ;
#6460 = DIRECTION ( 'NONE',  ( 0.8795363392562568494, -0.4758317222797389667, -4.707970883985391064E-16 ) ) ;
#6461 = ORIENTED_EDGE ( 'NONE', *, *, #1409, .T. ) ;
#6462 = CARTESIAN_POINT ( 'NONE',  ( 14.97072768011073940, -34.32654753528365177, 2.597518595105000383 ) ) ;
#6463 = CARTESIAN_POINT ( 'NONE',  ( -1.721951098409294945, -66.71030961465282871, -0.9872116442447198548 ) ) ;
#6464 = CARTESIAN_POINT ( 'NONE',  ( 6.643375263299909683, -62.64442119333418901, -2.502572238011808281 ) ) ;
#6465 = ORIENTED_EDGE ( 'NONE', *, *, #1153, .T. ) ;
#6466 = ADVANCED_FACE ( 'NONE', ( #4067 ), #2339, .F. ) ;
#6467 = DIRECTION ( 'NONE',  ( 1.000000000000000000, 0.000000000000000000, 0.000000000000000000 ) ) ;
#6468 = EDGE_CURVE ( 'NONE', #1675, #7067, #571, .T. ) ;
#6469 = CARTESIAN_POINT ( 'NONE',  ( 7.283874945971848369, -8.906884184084093548, -3.000000000000009770 ) ) ;
#6470 = DIRECTION ( 'NONE',  ( -0.1546180985661130547, 0.9879743132267154726, 9.870744795757317374E-16 ) ) ;
#6471 = LINE ( 'NONE', #4784, #5661 ) ;
#6472 = CARTESIAN_POINT ( 'NONE',  ( 0.000000000000000000, 0.000000000000000000, 3.500000000000000000 ) ) ;
#6473 = ADVANCED_FACE ( 'NONE', ( #1738 ), #7038, .F. ) ;
#6474 = CARTESIAN_POINT ( 'NONE',  ( 2.533447467746755333, -55.76293992159236979, -0.1309777151760100067 ) ) ;
#6475 = CARTESIAN_POINT ( 'NONE',  ( 26.13478801451176636, 24.75419629621026019, -1.493845543551509891 ) ) ;
#6476 = CARTESIAN_POINT ( 'NONE',  ( -0.8826897099904034150, -54.72534079625300052, 0.03922796265859054832 ) ) ;
#6477 = CARTESIAN_POINT ( 'NONE',  ( 6.493768279116130415, -62.63809584774485018, -3.239169643854469705 ) ) ;
#6478 = ORIENTED_EDGE ( 'NONE', *, *, #5189, .T. ) ;
#6479 = DIRECTION ( 'NONE',  ( -0.2467992669038191755, 0.02032136184815236737, 0.9688535307818070264 ) ) ;
#6480 = CIRCLE ( 'NONE', #7443, 0.7500000000000000000 ) ;
#6481 = CARTESIAN_POINT ( 'NONE',  ( 10.46182022341160867, 4.774967812772744402, 4.770489558936219510E-15 ) ) ;
#6482 = CARTESIAN_POINT ( 'NONE',  ( 17.79228376992792349, -39.86704927745797988, -0.6257137034768931461 ) ) ;
#6483 = CARTESIAN_POINT ( 'NONE',  ( 1.785462125252589960, -54.25404267560509908, 2.136629312307830375 ) ) ;
#6484 = CARTESIAN_POINT ( 'NONE',  ( -4.614416121558960526, -57.55752852796073427, -0.1302737383155048445 ) ) ;
#6485 = AXIS2_PLACEMENT_3D ( 'NONE', #4068, #3039, #110 ) ;
#6486 = LINE ( 'NONE', #7054, #5450 ) ;
#6487 = CARTESIAN_POINT ( 'NONE',  ( 15.08188723176695056, -33.99092340910145538, 5.072392329257909616 ) ) ;
#6488 = ORIENTED_EDGE ( 'NONE', *, *, #1862, .T. ) ;
#6489 = PRODUCT_DEFINITION ( 'UNKNOWN', '', #159, #5865 ) ;
#6490 = VERTEX_POINT ( 'NONE', #2370 ) ;
#6491 = VERTEX_POINT ( 'NONE', #5915 ) ;
#6492 = DIRECTION ( 'NONE',  ( 0.4039838799357178822, 0.9147661038495488173, -2.999999999999999208E-14 ) ) ;
#6493 = FACE_OUTER_BOUND ( 'NONE', #4357, .T. ) ;
#6494 = CARTESIAN_POINT ( 'NONE',  ( -1.435618805647706164, -65.69410370267330279, -0.7494494782121799981 ) ) ;
#6495 = CARTESIAN_POINT ( 'NONE',  ( 6.133675886466185112, -62.42807403084368900, -1.580205649328261241 ) ) ;
#6496 = CIRCLE ( 'NONE', #3973, 1.000000000000001110 ) ;
#6497 = EDGE_LOOP ( 'NONE', ( #6430, #5645, #4232, #5956 ) ) ;
#6498 = ADVANCED_FACE ( 'NONE', ( #5883 ), #5772, .T. ) ;
#6499 = ORIENTED_EDGE ( 'NONE', *, *, #5702, .F. ) ;
#6500 = EDGE_LOOP ( 'NONE', ( #1301, #4370, #5297, #7126, #2925, #3282 ) ) ;
#6501 = CARTESIAN_POINT ( 'NONE',  ( -31.91091272472834817, 16.82560631625344172, 0.006154456448481410852 ) ) ;
#6502 = CARTESIAN_POINT ( 'NONE',  ( 0.000000000000000000, 0.000000000000000000, -3.500000000000000000 ) ) ;
#6503 = DIRECTION ( 'NONE',  ( -5.715354789860003484E-18, -9.999836672264337477E-16, 1.000000000000000000 ) ) ;
#6504 = CARTESIAN_POINT ( 'NONE',  ( -5.628700163094269016, -63.23550210468251009, 3.461537593744290042 ) ) ;
#6505 = VERTEX_POINT ( 'NONE', #5204 ) ;
#6506 = EDGE_CURVE ( 'NONE', #555, #2243, #5587, .T. ) ;
#6507 = ADVANCED_FACE ( 'NONE', ( #6995, #4603 ), #3493, .T. ) ;
#6508 = VECTOR ( 'NONE', #6235, 1000.000000000000000 ) ;
#6509 = DIRECTION ( 'NONE',  ( -1.046706025223848628E-16, 1.111638688234981601E-15, -1.000000000000000000 ) ) ;
#6510 = CARTESIAN_POINT ( 'NONE',  ( -4.773669824303439668, -63.68048849998092464, 3.536592896228280214 ) ) ;
#6511 = DIRECTION ( 'NONE',  ( 0.000000000000000000, 0.000000000000000000, -1.000000000000000000 ) ) ;
#6512 = AXIS2_PLACEMENT_3D ( 'NONE', #4425, #6163, #437 ) ;
#6513 = DIRECTION ( 'NONE',  ( -0.9999836672264332815, 0.005715354789845002517, 0.000000000000000000 ) ) ;
#6514 = CARTESIAN_POINT ( 'NONE',  ( -1.329205950148755644, -54.81433347601338113, 0.01301773866004049540 ) ) ;
#6515 = ADVANCED_FACE ( 'NONE', ( #3038 ), #1840, .F. ) ;
#6516 = EDGE_LOOP ( 'NONE', ( #3854, #5475 ) ) ;
#6517 = MECHANICAL_DESIGN_GEOMETRIC_PRESENTATION_REPRESENTATION (  '', ( #1833 ), #2906 ) ;
#6518 = CARTESIAN_POINT ( 'NONE',  ( 27.30483170388656333, -34.44723004512044895, -3.427979277949995323E-14 ) ) ;
#6519 = TOROIDAL_SURFACE ( 'NONE', #5818, 1.500000000000000000, 1.000000000000000000 ) ;
#6520 = CIRCLE ( 'NONE', #4020, 140.0000000000000000 ) ;
#6521 = CARTESIAN_POINT ( 'NONE',  ( -19.94212619460463287, -40.63668738334721553, -3.000000000000041744 ) ) ;
#6522 = CYLINDRICAL_SURFACE ( 'NONE', #1844, 145.9999999999999716 ) ;
#6523 = AXIS2_PLACEMENT_3D ( 'NONE', #3524, #2281, #5731 ) ;
#6524 = DIRECTION ( 'NONE',  ( 0.9793199139485104787, 0.2023178344681509366, 2.079116908177630447E-16 ) ) ;
#6525 = CIRCLE ( 'NONE', #4374, 0.7500000000000000000 ) ;
#6526 = CARTESIAN_POINT ( 'NONE',  ( -3.235261603508409856, -66.01500717273368934, 1.164464255201294929 ) ) ;
#6527 = DIRECTION ( 'NONE',  ( 0.2223191033124283789, 0.6712482523644727195, 0.7071067811865466846 ) ) ;
#6528 = ORIENTED_EDGE ( 'NONE', *, *, #6379, .T. ) ;
#6529 = VECTOR ( 'NONE', #5546, 1000.000000000000227 ) ;
#6530 = ORIENTED_EDGE ( 'NONE', *, *, #3324, .F. ) ;
#6531 = EDGE_LOOP ( 'NONE', ( #3350, #4785, #4720, #2161 ) ) ;
#6532 = ORIENTED_EDGE ( 'NONE', *, *, #3456, .T. ) ;
#6533 = VECTOR ( 'NONE', #3173, 1000.000000000000000 ) ;
#6534 = CYLINDRICAL_SURFACE ( 'NONE', #4623, 0.9999999999999980016 ) ;
#6535 = CIRCLE ( 'NONE', #5228, 1.000000000000001776 ) ;
#6536 = CARTESIAN_POINT ( 'NONE',  ( 43.95483829995806957, -94.87490738911687060, 2.999999999999905409 ) ) ;
#6537 = CARTESIAN_POINT ( 'NONE',  ( 3.594547628745600409, -65.86039197651267330, -3.372550074330296965 ) ) ;
#6538 = VERTEX_POINT ( 'NONE', #4179 ) ;
#6539 = AXIS2_PLACEMENT_3D ( 'NONE', #2684, #1032, #3883 ) ;
#6540 = ORIENTED_EDGE ( 'NONE', *, *, #3107, .F. ) ;
#6541 = EDGE_LOOP ( 'NONE', ( #1120, #5678, #2657, #1265 ) ) ;
#6542 =( REPRESENTATION_RELATIONSHIP ('NONE','NONE', #3195, #5284 ) REPRESENTATION_RELATIONSHIP_WITH_TRANSFORMATION ( #4021 )SHAPE_REPRESENTATION_RELATIONSHIP( ) );
#6543 = CARTESIAN_POINT ( 'NONE',  ( -22.27644891976294161, 9.837844043328894728, -2.993845543551559629 ) ) ;
#6544 = EDGE_CURVE ( 'NONE', #6210, #6869, #2078, .T. ) ;
#6545 = DIRECTION ( 'NONE',  ( -0.9999836672264333925, 0.005715354789844984303, 0.000000000000000000 ) ) ;
#6546 = CIRCLE ( 'NONE', #1966, 5.000000000000000000 ) ;
#6547 = DIRECTION ( 'NONE',  ( -0.6713653717953970146, 0.7411265327553913096, 7.927884880413787584E-16 ) ) ;
#6548 = CARTESIAN_POINT ( 'NONE',  ( -6.026198395890769888, -63.94474587426248036, 1.222360836057740041 ) ) ;
#6549 = ORIENTED_EDGE ( 'NONE', *, *, #38, .T. ) ;
#6550 = ORIENTED_EDGE ( 'NONE', *, *, #659, .T. ) ;
#6551 = PRESENTATION_STYLE_ASSIGNMENT (( #4078 ) ) ;
#6552 = CARTESIAN_POINT ( 'NONE',  ( 2.799893819535080208, -55.23287331081275653, 0.2233987335540700003 ) ) ;
#6553 = ADVANCED_FACE ( 'NONE', ( #6961 ), #1956, .T. ) ;
#6554 = DIRECTION ( 'NONE',  ( -0.9999836672264333925, 0.005715354789844476896, 0.000000000000000000 ) ) ;
#6555 = EDGE_CURVE ( 'NONE', #4778, #7025, #7253, .T. ) ;
#6556 = CARTESIAN_POINT ( 'NONE',  ( -6.629462435860018488, -62.64420580508557634, 2.974566524362353803 ) ) ;
#6557 = CARTESIAN_POINT ( 'NONE',  ( 5.463696144088109996, -62.30361170774578028, -3.475027489484119769 ) ) ;
#6558 = VERTEX_POINT ( 'NONE', #4323 ) ;
#6559 = CARTESIAN_POINT ( 'NONE',  ( -13.49899450467539985, -35.75040780681265318, -2.566271404894997499 ) ) ;
#6560 = ADVANCED_FACE ( 'NONE', ( #1979 ), #2051, .T. ) ;
#6561 = DIRECTION ( 'NONE',  ( 5.715354789845005112E-18, 9.999836672264339449E-16, -1.000000000000000000 ) ) ;
#6562 = CARTESIAN_POINT ( 'NONE',  ( -28.68093632328499965, 11.79168739492699913, -1.500000000001999956 ) ) ;
#6563 = CARTESIAN_POINT ( 'NONE',  ( -5.714251477591489881, -57.46902543231049521, -0.4259505751857597389 ) ) ;
#6564 = CARTESIAN_POINT ( 'NONE',  ( -2.148471732745839802, -67.07461398899560834, 3.078016402823839925 ) ) ;
#6565 = CARTESIAN_POINT ( 'NONE',  ( -14.02739156872318027, -37.17434273187110705, -0.4662714048949997969 ) ) ;
#6566 = ORIENTED_EDGE ( 'NONE', *, *, #4686, .F. ) ;
#6567 = ORIENTED_EDGE ( 'NONE', *, *, #2863, .T. ) ;
#6568 = PRODUCT_DEFINITION_SHAPE ( 'NONE', 'NONE',  #6489 ) ;
#6569 = CARTESIAN_POINT ( 'NONE',  ( -105.7473861751082040, -118.0666774205683822, -1.186117176699141851E-13 ) ) ;
#6570 = ADVANCED_FACE ( 'NONE', ( #2014 ), #299, .T. ) ;
#6571 = DIRECTION ( 'NONE',  ( 0.8056443796264692869, -0.5923994712829185882, -5.877852522924713037E-16 ) ) ;
#6572 = CARTESIAN_POINT ( 'NONE',  ( -4.461725341067024786, -62.58642870417541104, 2.208339520507450082 ) ) ;
#6573 = CARTESIAN_POINT ( 'NONE',  ( -0.01776538050268356914, -54.19622611322429862, -0.06040963844522982684 ) ) ;
#6574 = ORIENTED_EDGE ( 'NONE', *, *, #5421, .T. ) ;
#6575 = ORIENTED_EDGE ( 'NONE', *, *, #750, .F. ) ;
#6576 = APPLICATION_PROTOCOL_DEFINITION ( 'draft international standard', 'automotive_design', 1998, #5258 ) ;
#6577 = PLANE ( 'NONE',  #1250 ) ;
#6578 = DIRECTION ( 'NONE',  ( 0.000000000000000000, 0.000000000000000000, -1.000000000000000000 ) ) ;
#6579 = DIRECTION ( 'NONE',  ( -0.2467992669038191478, 0.02032136184815930280, 0.9688535307818069153 ) ) ;
#6580 = CARTESIAN_POINT ( 'NONE',  ( -3.403807323753265113, -54.36107883567960641, 1.752763223655470437 ) ) ;
#6581 = ORIENTED_EDGE ( 'NONE', *, *, #6642, .T. ) ;
#6582 = EDGE_CURVE ( 'NONE', #507, #3517, #6614, .T. ) ;
#6583 = CARTESIAN_POINT ( 'NONE',  ( -105.7473861751082040, -118.0666774205683822, -1.188285581044112860E-13 ) ) ;
#6584 = CARTESIAN_POINT ( 'NONE',  ( 5.010558598472139913, -57.30068827582834956, 0.4001341763009204078 ) ) ;
#6585 = SURFACE_STYLE_USAGE ( .BOTH. , #5392 ) ;
#6586 = CARTESIAN_POINT ( 'NONE',  ( -5.904042796847299712, -62.42803713013675093, 3.506543003539000392 ) ) ;
#6587 = CARTESIAN_POINT ( 'NONE',  ( 5.724602046902682595, -59.58971228651716245, -1.534163154136720442 ) ) ;
#6588 = ORIENTED_EDGE ( 'NONE', *, *, #5198, .T. ) ;
#6589 = B_SPLINE_CURVE_WITH_KNOTS ( 'NONE', 3,
 ( #7389, #3808, #2645, #468 ),
 .UNSPECIFIED., .F., .F.,
 ( 4, 4 ),
 ( 0.000000000000000000, 1.000000000000000000 ),
 .UNSPECIFIED. ) ;
#6590 = DIRECTION ( 'NONE',  ( -0.9492899500389725409, -0.3144019573014856794, 0.000000000000000000 ) ) ;
#6591 = DIRECTION ( 'NONE',  ( 0.9492883822130744331, -0.3144066910790611624, 0.000000000000000000 ) ) ;
#6592 = DIRECTION ( 'NONE',  ( 0.000000000000000000, 1.000000000000000000, 1.734723475976805517E-15 ) ) ;
#6593 = PLANE ( 'NONE',  #1129 ) ;
#6594 = CARTESIAN_POINT ( 'NONE',  ( -1.206827191127304078, -66.77204028133226643, -1.044217440639481742 ) ) ;
#6595 = CARTESIAN_POINT ( 'NONE',  ( 1.944327905822930136, -53.75057748617523856, 2.017748614706070143 ) ) ;
#6596 = FACE_OUTER_BOUND ( 'NONE', #3953, .T. ) ;
#6597 = VERTEX_POINT ( 'NONE', #4290 ) ;
#6598 = EDGE_CURVE ( 'NONE', #4300, #3483, #3758, .T. ) ;
#6599 = EDGE_CURVE ( 'NONE', #5920, #2243, #4862, .T. ) ;
#6600 = ORIENTED_EDGE ( 'NONE', *, *, #2322, .F. ) ;
#6601 = DIRECTION ( 'NONE',  ( 5.715354789845005112E-18, 9.999836672264339449E-16, -1.000000000000000000 ) ) ;
#6602 = AXIS2_PLACEMENT_3D ( 'NONE', #7187, #6666, #2562 ) ;
#6603 = CARTESIAN_POINT ( 'NONE',  ( 7.529070345495034289, 16.11642554373086256, 1.604619215278546562E-14 ) ) ;
#6604 = CARTESIAN_POINT ( 'NONE',  ( -5.227302941343250353, -58.92678856866081105, -0.2192372590660296439 ) ) ;
#6605 = DIRECTION ( 'NONE',  ( -0.2467992669038191478, 0.02032136184815930280, 0.9688535307818069153 ) ) ;
#6606 = CARTESIAN_POINT ( 'NONE',  ( -0.8961004093985418528, -66.62686089995901284, 3.138778905044528500 ) ) ;
#6607 = EDGE_LOOP ( 'NONE', ( #508, #5415, #6973, #3319, #3943, #6600 ) ) ;
#6608 = ORIENTED_EDGE ( 'NONE', *, *, #4679, .F. ) ;
#6609 = VERTEX_POINT ( 'NONE', #2591 ) ;
#6610 = CIRCLE ( 'NONE', #1909, 1.000000000000000888 ) ;
#6611 = DIRECTION ( 'NONE',  ( -5.715354789845005112E-18, -9.999836672264339449E-16, 1.000000000000000000 ) ) ;
#6612 = CARTESIAN_POINT ( 'NONE',  ( 0.000000000000000000, 0.000000000000000000, 3.000000000000000000 ) ) ;
#6613 = CIRCLE ( 'NONE', #6031, 7.844444444444450326 ) ;
#6614 = LINE ( 'NONE', #2624, #3157 ) ;
#6615 = CARTESIAN_POINT ( 'NONE',  ( -6.822623972396280934, -59.02239909983155286, -0.6330850349556997880 ) ) ;
#6616 = ORIENTED_EDGE ( 'NONE', *, *, #750, .T. ) ;
#6617 = ORIENTED_EDGE ( 'NONE', *, *, #1093, .T. ) ;
#6618 = CIRCLE ( 'NONE', #5551, 1.000000000000001776 ) ;
#6619 = FACE_OUTER_BOUND ( 'NONE', #5375, .T. ) ;
#6620 = CARTESIAN_POINT ( 'NONE',  ( -5.595710845088040841, -61.75488600311453524, 3.658668618637090031 ) ) ;
#6621 = ORIENTED_EDGE ( 'NONE', *, *, #2475, .F. ) ;
#6622 = DIRECTION ( 'NONE',  ( 5.715354789860003484E-18, 9.999836672264337477E-16, -1.000000000000000000 ) ) ;
#6623 = CARTESIAN_POINT ( 'NONE',  ( 9.154985593248634146, -46.96141903535870910, -4.683753385137379155E-14 ) ) ;
#6624 = VERTEX_POINT ( 'NONE', #2480 ) ;
#6625 = FACE_OUTER_BOUND ( 'NONE', #785, .T. ) ;
#6626 = DIRECTION ( 'NONE',  ( 5.715354789845005112E-18, 9.999836672264339449E-16, -1.000000000000000000 ) ) ;
#6627 = CARTESIAN_POINT ( 'NONE',  ( -33.94153943842304955, 12.25650441806195801, -2.999999999999988898 ) ) ;
#6628 = EDGE_CURVE ( 'NONE', #716, #2186, #6075, .T. ) ;
#6629 = CARTESIAN_POINT ( 'NONE',  ( 6.645018675491529692, -62.64496150164843158, -2.502481404895003259 ) ) ;
#6630 = DIRECTION ( 'NONE',  ( 0.2164621326156030423, -0.07169280077033016174, 0.9736551173085935540 ) ) ;
#6631 = CARTESIAN_POINT ( 'NONE',  ( -3.773574383489684880, -54.58470482469731877, -0.3679774332281250393 ) ) ;
#6632 = DIRECTION ( 'NONE',  ( 0.9999836672264332815, -0.005715354789847320975, 0.000000000000000000 ) ) ;
#6633 = AXIS2_PLACEMENT_3D ( 'NONE', #6475, #5315, #682 ) ;
#6634 = EDGE_LOOP ( 'NONE', ( #292, #1496, #2586, #2121, #6982, #2759 ) ) ;
#6635 = ORIENTED_EDGE ( 'NONE', *, *, #3518, .T. ) ;
#6636 = ORIENTED_EDGE ( 'NONE', *, *, #668, .F. ) ;
#6637 = DIRECTION ( 'NONE',  ( -0.9999836672264332815, 0.005715354789859876036, 0.000000000000000000 ) ) ;
#6638 = CIRCLE ( 'NONE', #3395, 0.7499999999999893419 ) ;
#6639 = CIRCLE ( 'NONE', #3628, 0.5000000000000004441 ) ;
#6640 = DIRECTION ( 'NONE',  ( 0.2223157560262039867, -0.6712493609847990372, 0.7071067811865450192 ) ) ;
#6641 = EDGE_CURVE ( 'NONE', #7283, #1942, #4783, .T. ) ;
#6642 = EDGE_CURVE ( 'NONE', #3409, #1452, #4365, .T. ) ;
#6643 = CARTESIAN_POINT ( 'NONE',  ( -6.217266535765080704, -62.33106447713396392, -2.754524245347104383 ) ) ;
#6644 = DIRECTION ( 'NONE',  ( 5.715354789845005112E-18, 9.999836672264339449E-16, -1.000000000000000000 ) ) ;
#6645 = CARTESIAN_POINT ( 'NONE',  ( 2.014066015375293617, -66.41055546370263585, 2.981310916594474225 ) ) ;
#6646 = AXIS2_PLACEMENT_3D ( 'NONE', #590, #560, #2878 ) ;
#6647 = ORIENTED_EDGE ( 'NONE', *, *, #4805, .T. ) ;
#6648 = ORIENTED_EDGE ( 'NONE', *, *, #2674, .T. ) ;
#6649 = VECTOR ( 'NONE', #1237, 1000.000000000000000 ) ;
#6650 = PRODUCT_DEFINITION_FORMATION_WITH_SPECIFIED_SOURCE ( 'ANY', '', #6392, .NOT_KNOWN. ) ;
#6651 = VECTOR ( 'NONE', #5424, 999.9999999999998863 ) ;
#6652 = SHAPE_REPRESENTATION_RELATIONSHIP ( 'NONE' , 'NONE' ,  #7047, #5592 ) ;
#6653 = DIRECTION ( 'NONE',  ( -0.9999836672264333925, 0.005715354789845005987, 4.554564057672517313E-33 ) ) ;
#6654 = TOROIDAL_SURFACE ( 'NONE', #5100, 1.500000000000000000, 1.000000000000000000 ) ;
#6655 = EDGE_CURVE ( 'NONE', #3815, #6686, #3530, .T. ) ;
#6656 = CARTESIAN_POINT ( 'NONE',  ( 27.68174825049008803, -37.24611774345110149, -3.001370543551577619 ) ) ;
#6657 = CARTESIAN_POINT ( 'NONE',  ( 43.89994888609457035, -93.87291691326068133, -3.001370543551634018 ) ) ;
#6658 = CARTESIAN_POINT ( 'NONE',  ( -5.714251477591489881, -57.46902543231049521, -0.4259505751857597389 ) ) ;
#6659 = ORIENTED_EDGE ( 'NONE', *, *, #1071, .F. ) ;
#6660 = AXIS2_PLACEMENT_3D ( 'NONE', #3054, #4759, #1369 ) ;
#6661 = AXIS2_PLACEMENT_3D ( 'NONE', #4968, #700, #6397 ) ;
#6662 = VERTEX_POINT ( 'NONE', #3185 ) ;
#6663 = CARTESIAN_POINT ( 'NONE',  ( 39.97800414936823188, -95.26063634933134949, -3.001370543551635794 ) ) ;
#6664 = CARTESIAN_POINT ( 'NONE',  ( -1.206827191127304078, -66.77204028133226643, -1.044217440639481742 ) ) ;
#6665 = AXIS2_PLACEMENT_3D ( 'NONE', #4383, #5521, #1139 ) ;
#6666 = DIRECTION ( 'NONE',  ( -5.715354789845005112E-18, -9.999836672264339449E-16, 1.000000000000000000 ) ) ;
#6667 = CARTESIAN_POINT ( 'NONE',  ( 10.02759472486470926, 5.630039434485818894, -2.999999999999995115 ) ) ;
#6668 = ORIENTED_EDGE ( 'NONE', *, *, #749, .T. ) ;
#6669 = CYLINDRICAL_SURFACE ( 'NONE', #7349, 5.000000000000000000 ) ;
#6670 = DIRECTION ( 'NONE',  ( 1.850371707708594760E-14, 4.625929269271487058E-14, -1.000000000000000000 ) ) ;
#6671 = CARTESIAN_POINT ( 'NONE',  ( -9.358272925367041140, -51.27205205187813419, 2.526284428608170263 ) ) ;
#6672 = PRODUCT_DEFINITION_CONTEXT ( 'detailed design', #6403, 'design' ) ;
#6673 = B_SPLINE_CURVE_WITH_KNOTS ( 'NONE', 3,
 ( #584, #515, #2754, #6241, #3327, #474 ),
 .UNSPECIFIED., .F., .F.,
 ( 4, 2, 4 ),
 ( 0.000000000000000000, 0.0003938972045929564408, 0.0007877944091859128816 ),
 .UNSPECIFIED. ) ;
#6674 = CARTESIAN_POINT ( 'NONE',  ( 9.389618828306289799, -51.17759410398493714, -3.490074380419979860 ) ) ;
#6675 = CARTESIAN_POINT ( 'NONE',  ( -105.7473861751082040, -118.0666774205683822, 2.999999999999881428 ) ) ;
#6676 = CARTESIAN_POINT ( 'NONE',  ( -6.093803043304910183, -63.45548452497258296, 3.342215352752540447 ) ) ;
#6677 = FACE_OUTER_BOUND ( 'NONE', #4245, .T. ) ;
#6678 = VERTEX_POINT ( 'NONE', #5511 ) ;
#6679 = VERTEX_POINT ( 'NONE', #334 ) ;
#6680 = EDGE_CURVE ( 'NONE', #6736, #5506, #4933, .T. ) ;
#6681 = CARTESIAN_POINT ( 'NONE',  ( -13.76286933773225130, 13.32929763200878881, -0.3999035282155013471 ) ) ;
#6682 = DIRECTION ( 'NONE',  ( -0.8688689365825379429, -0.4950421911735701230, -3.889776975374848285E-16 ) ) ;
#6683 = CARTESIAN_POINT ( 'NONE',  ( 1.080279179814437773, -65.65553934942860792, 2.784998920779040432 ) ) ;
#6684 = DIRECTION ( 'NONE',  ( 0.9999836672264332815, -0.005715354789845002517, 0.000000000000000000 ) ) ;
#6685 = CARTESIAN_POINT ( 'NONE',  ( 6.248302252609925667, -60.41094430931507020, 0.4638711834344099727 ) ) ;
#6686 = VERTEX_POINT ( 'NONE', #3710 ) ;
#6687 = CARTESIAN_POINT ( 'NONE',  ( -5.172139827190740391, -61.55016382346040871, 1.714186298074440007 ) ) ;
#6688 = ORIENTED_EDGE ( 'NONE', *, *, #1986, .F. ) ;
#6689 = VERTEX_POINT ( 'NONE', #257 ) ;
#6690 = ORIENTED_EDGE ( 'NONE', *, *, #5399, .T. ) ;
#6691 = APPLICATION_PROTOCOL_DEFINITION ( 'draft international standard', 'automotive_design', 1998, #3312 ) ;
#6692 = DIRECTION ( 'NONE',  ( -5.715354789860003484E-18, -9.999836672264337477E-16, 1.000000000000000000 ) ) ;
#6693 = CARTESIAN_POINT ( 'NONE',  ( 38.49686355599224896, -95.49243502991532750, 3.999999999999904521 ) ) ;
#6694 = CARTESIAN_POINT ( 'NONE',  ( 0.000000000000000000, 0.000000000000000000, -2.544444444444450060 ) ) ;
#6695 = CARTESIAN_POINT ( 'NONE',  ( -1.626396133375414887, -53.66552156771879112, 1.839959185157149957 ) ) ;
#6696 = EDGE_LOOP ( 'NONE', ( #3707, #392, #5901, #3634 ) ) ;
#6697 = ORIENTED_EDGE ( 'NONE', *, *, #6966, .T. ) ;
#6698 = ORIENTED_EDGE ( 'NONE', *, *, #3003, .F. ) ;
#6699 = ADVANCED_FACE ( 'NONE', ( #6032 ), #5342, .F. ) ;
#6700 = ADVANCED_FACE ( 'NONE', ( #933 ), #3676, .F. ) ;
#6701 = DIRECTION ( 'NONE',  ( -0.9492883822130744331, 0.3144066910790611624, 0.000000000000000000 ) ) ;
#6702 = CARTESIAN_POINT ( 'NONE',  ( 2.080482015124565098, -66.54183146390657555, -1.221303033644861813 ) ) ;
#6703 = DIRECTION ( 'NONE',  ( 0.9147661038495488173, -0.4039838799357178822, 0.000000000000000000 ) ) ;
#6704 = DIRECTION ( 'NONE',  ( 0.6513146796332652810, 0.5900073775824578037, -0.4771587602596099598 ) ) ;
#6705 = ORIENTED_EDGE ( 'NONE', *, *, #4592, .T. ) ;
#6706 = EDGE_CURVE ( 'NONE', #2728, #4894, #1134, .T. ) ;
#6707 = CARTESIAN_POINT ( 'NONE',  ( 14.49911764349215915, -35.75048010860329839, 0.4975185951050001831 ) ) ;
#6708 = FACE_OUTER_BOUND ( 'NONE', #6036, .T. ) ;
#6709 = CARTESIAN_POINT ( 'NONE',  ( 6.696612653858620590, -58.50870383553881737, 0.2496331057155200817 ) ) ;
#6710 = DIRECTION ( 'NONE',  ( 0.000000000000000000, 0.000000000000000000, -1.000000000000000000 ) ) ;
#6711 = ORIENTED_EDGE ( 'NONE', *, *, #6192, .T. ) ;
#6712 = EDGE_LOOP ( 'NONE', ( #4126, #1378, #4070, #6659 ) ) ;
#6713 = LINE ( 'NONE', #6017, #4250 ) ;
#6714 = FACE_OUTER_BOUND ( 'NONE', #3099, .T. ) ;
#6715 = CARTESIAN_POINT ( 'NONE',  ( 2.467202665543605011, -65.15865635802147438, 2.695445654378740397 ) ) ;
#6716 = LINE ( 'NONE', #325, #981 ) ;
#6717 = CARTESIAN_POINT ( 'NONE',  ( 0.9768556859363289879, -66.61496767163153265, -1.161982190194281062 ) ) ;
#6718 = ORIENTED_EDGE ( 'NONE', *, *, #419, .F. ) ;
#6719 = ORIENTED_EDGE ( 'NONE', *, *, #4473, .T. ) ;
#6720 = ORIENTED_EDGE ( 'NONE', *, *, #2769, .T. ) ;
#6721 = CIRCLE ( 'NONE', #1081, 141.0000000000000284 ) ;
#6722 = DIRECTION ( 'NONE',  ( 0.9492883822130744331, -0.3144066910790611624, 0.000000000000000000 ) ) ;
#6723 = CARTESIAN_POINT ( 'NONE',  ( 27.68174825049008803, -37.24611774345110149, -3.001370543551577619 ) ) ;
#6724 = DIRECTION ( 'NONE',  ( 0.9999836672264331705, -0.005715354789860001804, 0.000000000000000000 ) ) ;
#6725 = FACE_OUTER_BOUND ( 'NONE', #696, .T. ) ;
#6726 = EDGE_CURVE ( 'NONE', #5349, #2665, #1205, .T. ) ;
#6727 = CIRCLE ( 'NONE', #599, 11.50000000000000178 ) ;
#6728 = CYLINDRICAL_SURFACE ( 'NONE', #4839, 1.000000000000001332 ) ;
#6729 = CARTESIAN_POINT ( 'NONE',  ( -28.37794841333281681, 12.47776197281474708, -1.499999999999988010 ) ) ;
#6730 = CARTESIAN_POINT ( 'NONE',  ( 5.465222000274489567, -57.03231251543625291, 0.2812537129946697800 ) ) ;
#6731 = VECTOR ( 'NONE', #3392, 1000.000000000000000 ) ;
#6732 = DIRECTION ( 'NONE',  ( -0.4758317222797389667, -0.8795363392562568494, -8.822415211014833627E-16 ) ) ;
#6733 = EDGE_CURVE ( 'NONE', #6854, #6928, #453, .T. ) ;
#6734 = EDGE_CURVE ( 'NONE', #2855, #2713, #3647, .T. ) ;
#6735 = DIRECTION ( 'NONE',  ( -5.715354789860003484E-18, -9.999836672264337477E-16, 1.000000000000000000 ) ) ;
#6736 = VERTEX_POINT ( 'NONE', #6178 ) ;
#6737 = CIRCLE ( 'NONE', #2409, 7.844444444444450326 ) ;
#6738 = ORIENTED_EDGE ( 'NONE', *, *, #3504, .F. ) ;
#6739 = DIRECTION ( 'NONE',  ( -0.9492883822130750993, 0.3144066910790586089, 0.000000000000000000 ) ) ;
#6740 = DIRECTION ( 'NONE',  ( 0.000000000000000000, 0.000000000000000000, 1.000000000000000000 ) ) ;
#6741 = ADVANCED_FACE ( 'NONE', ( #968, #3904 ), #2249, .F. ) ;
#6742 = DIRECTION ( 'NONE',  ( -0.6713653717953991240, 0.7411265327553895332, 8.112475779533124710E-16 ) ) ;
#6743 = CARTESIAN_POINT ( 'NONE',  ( -2.113079283527464991, -53.41662231759018198, -0.8523026345115048974 ) ) ;
#6744 = CARTESIAN_POINT ( 'NONE',  ( 14.63763862841553376, 20.11382921380833011, -2.993845543551509447 ) ) ;
#6745 = VERTEX_POINT ( 'NONE', #5576 ) ;
#6746 = CARTESIAN_POINT ( 'NONE',  ( 12.34225220476766438, -34.27182074065601114, -3.426078865054194011E-14 ) ) ;
#6747 = CARTESIAN_POINT ( 'NONE',  ( 4.485945982887084682, -58.07227379738043993, 1.147183751133595386 ) ) ;
#6748 = DIRECTION ( 'NONE',  ( -0.06375834441969779887, -0.9979653668924884924, -9.983134689092966662E-16 ) ) ;
#6749 = DIRECTION ( 'NONE',  ( -5.715354789860003484E-18, -9.999836672264337477E-16, 1.000000000000000000 ) ) ;
#6750 = AXIS2_PLACEMENT_3D ( 'NONE', #6864, #3361, #2236 ) ;
#6751 = CARTESIAN_POINT ( 'NONE',  ( 1.460134286533229853, -55.58368472982129305, 0.8822880931559249351 ) ) ;
#6752 = AXIS2_PLACEMENT_3D ( 'NONE', #3378, #5130, #7409 ) ;
#6753 = DIRECTION ( 'NONE',  ( -5.715354789860003484E-18, -9.999836672264337477E-16, 1.000000000000000000 ) ) ;
#6754 = CARTESIAN_POINT ( 'NONE',  ( -105.7473861751082040, -118.0666774205683822, -1.188285581044112860E-13 ) ) ;
#6755 = VERTEX_POINT ( 'NONE', #2765 ) ;
#6756 = VERTEX_POINT ( 'NONE', #5078 ) ;
#6757 = VERTEX_POINT ( 'NONE', #6805 ) ;
#6758 = CIRCLE ( 'NONE', #3514, 5.000000000000000000 ) ;
#6759 = CARTESIAN_POINT ( 'NONE',  ( -44.78727511552453677, -94.39397278840091587, -3.001000000000095813 ) ) ;
#6760 = ORIENTED_EDGE ( 'NONE', *, *, #3518, .F. ) ;
#6761 = LINE ( 'NONE', #3337, #2442 ) ;
#6762 = CARTESIAN_POINT ( 'NONE',  ( 18.06432739836633061, -39.71205113188396041, -3.955074325938771262E-14 ) ) ;
#6763 = CARTESIAN_POINT ( 'NONE',  ( 7.124841322228030904, -62.19900605811294980, -0.1440571144897197509 ) ) ;
#6764 = ORIENTED_EDGE ( 'NONE', *, *, #5045, .F. ) ;
#6765 = AXIS2_PLACEMENT_3D ( 'NONE', #6462, #2987, #806 ) ;
#6766 = EDGE_LOOP ( 'NONE', ( #4531, #770, #2976, #4156 ) ) ;
#6767 = CARTESIAN_POINT ( 'NONE',  ( 26.87031364676134970, -34.69479876584121314, 3.499999999999965361 ) ) ;
#6768 = EDGE_CURVE ( 'NONE', #5062, #6869, #6142, .T. ) ;
#6769 = DIRECTION ( 'NONE',  ( -0.8688689365825387201, -0.4950421911735688463, -4.999999999999992500E-16 ) ) ;
#6770 = VECTOR ( 'NONE', #5832, 1000.000000000000000 ) ;
#6771 = CARTESIAN_POINT ( 'NONE',  ( 3.371673436877395069, -65.30458424753078361, -1.190358958913985798 ) ) ;
#6772 = AXIS2_PLACEMENT_3D ( 'NONE', #4921, #7167, #5529 ) ;
#6773 = AXIS2_PLACEMENT_3D ( 'NONE', #1152, #6971, #4719 ) ;
#6774 = DIRECTION ( 'NONE',  ( -0.9999836672264335036, 0.005715354789845008589, 0.000000000000000000 ) ) ;
#6775 = CARTESIAN_POINT ( 'NONE',  ( 19.34585819626726533, -40.86123582061801329, -4.076600168545496672E-14 ) ) ;
#6776 = ORIENTED_EDGE ( 'NONE', *, *, #3974, .F. ) ;
#6777 = APPLICATION_CONTEXT ( 'automotive_design' ) ;
#6778 = EDGE_CURVE ( 'NONE', #5943, #89, #1015, .T. ) ;
#6779 = ADVANCED_FACE ( 'NONE', ( #6725 ), #2809, .T. ) ;
#6780 = CARTESIAN_POINT ( 'NONE',  ( -17.04733905648494030, -8.234069079964157822, -3.000000000000009326 ) ) ;
#6781 = FACE_OUTER_BOUND ( 'NONE', #2423, .T. ) ;
#6782 = DIRECTION ( 'NONE',  ( -0.9999836672264332815, 0.005715354789859876036, 0.000000000000000000 ) ) ;
#6783 = CIRCLE ( 'NONE', #3281, 11.50000000000000178 ) ;
#6784 = CARTESIAN_POINT ( 'NONE',  ( 2.327488905229944560, -67.40324771348248589, -1.912586833593244773 ) ) ;
#6785 = LINE ( 'NONE', #6821, #2083 ) ;
#6786 = EDGE_LOOP ( 'NONE', ( #1099, #5536, #6532, #1206 ) ) ;
#6787 = DIRECTION ( 'NONE',  ( -5.715354789845005112E-18, -9.999836672264339449E-16, 1.000000000000000000 ) ) ;
#6788 = ADVANCED_FACE ( 'NONE', ( #413 ), #3302, .T. ) ;
#6789 = EDGE_CURVE ( 'NONE', #1992, #5998, #7260, .T. ) ;
#6790 = CARTESIAN_POINT ( 'NONE',  ( -4.653276882800380321, -62.74377975942224595, 3.226317067983300202 ) ) ;
#6791 = CARTESIAN_POINT ( 'NONE',  ( 18.06051344111304857, -40.30941759226211474, -0.6146628003278669095 ) ) ;
#6792 = CARTESIAN_POINT ( 'NONE',  ( 41.70778007397900211, -94.98992620957551480, -9.454242944073598665E-14 ) ) ;
#6793 = CARTESIAN_POINT ( 'NONE',  ( -4.882243101556620779, -59.05916974321930724, 0.3521297881290503806 ) ) ;
#6794 = CYLINDRICAL_SURFACE ( 'NONE', #6058, 2.999999999999999556 ) ;
#6795 = PLANE ( 'NONE',  #2764 ) ;
#6796 = ORIENTED_EDGE ( 'NONE', *, *, #5101, .F. ) ;
#6797 = CARTESIAN_POINT ( 'NONE',  ( -1.756031117750795234, -65.59594772693552045, 1.371125244074580030 ) ) ;
#6798 = ORIENTED_EDGE ( 'NONE', *, *, #619, .T. ) ;
#6799 = ORIENTED_EDGE ( 'NONE', *, *, #6221, .T. ) ;
#6800 = ORIENTED_EDGE ( 'NONE', *, *, #4995, .F. ) ;
#6801 = CARTESIAN_POINT ( 'NONE',  ( 4.492111197601039052, 14.38610368760445191, 3.000000000000014211 ) ) ;
#6802 = ORIENTED_EDGE ( 'NONE', *, *, #4152, .T. ) ;
#6803 = CARTESIAN_POINT ( 'NONE',  ( -32.93157973858376408, 14.54341967768581867, -2.999999999999986677 ) ) ;
#6804 = CARTESIAN_POINT ( 'NONE',  ( 27.99155020439383890, -34.64269665048639979, 2.999999999999965805 ) ) ;
#6805 = CARTESIAN_POINT ( 'NONE',  ( -8.362056880804429326, -51.09933645781752887, 2.533728595105000370 ) ) ;
#6806 = CARTESIAN_POINT ( 'NONE',  ( 6.281284389406939894, -57.15453665621128465, 0.6930907858711948810 ) ) ;
#6807 = ORIENTED_EDGE ( 'NONE', *, *, #5599, .T. ) ;
#6808 = ORIENTED_EDGE ( 'NONE', *, *, #7043, .F. ) ;
#6809 = CARTESIAN_POINT ( 'NONE',  ( -14.85943956261452037, -34.66209756224660055, -2.919824795488267455 ) ) ;
#6810 = CARTESIAN_POINT ( 'NONE',  ( -6.199032880790720235, -61.56120177486793210, 3.556545127952429830 ) ) ;
#6811 = CARTESIAN_POINT ( 'NONE',  ( -3.749938752099124972, 0.02143258046191922131, 3.000000000000000000 ) ) ;
#6812 = CARTESIAN_POINT ( 'NONE',  ( 27.96885038066250573, -34.65533836771933096, 3.261638044264441039 ) ) ;
#6813 = DIRECTION ( 'NONE',  ( 0.9979653668924883814, -0.06375834441969779887, -5.805357692931203648E-17 ) ) ;
#6814 = ORIENTED_CLOSED_SHELL ( 'NONE', *, #3500, .F. );
#6815 = ORIENTED_EDGE ( 'NONE', *, *, #1569, .T. ) ;
#6816 = DIRECTION ( 'NONE',  ( -5.715354789845005112E-18, -9.999836672264339449E-16, 1.000000000000000000 ) ) ;
#6817 = CARTESIAN_POINT ( 'NONE',  ( -15.00216760413269945, 6.625337177075938833, -3.299999999999993161 ) ) ;
#6818 = B_SPLINE_CURVE_WITH_KNOTS ( 'NONE', 3,
 ( #1763, #2958, #6952, #1830 ),
 .UNSPECIFIED., .F., .F.,
 ( 4, 4 ),
 ( 0.000000000000000000, 1.000000000000000000 ),
 .UNSPECIFIED. ) ;
#6819 = DIRECTION ( 'NONE',  ( -0.08966155106958693943, -0.9959722919136836383, 0.000000000000000000 ) ) ;
#6820 = CARTESIAN_POINT ( 'NONE',  ( -6.776085205154060986, -62.52991726716069820, -2.400146893717961749 ) ) ;
#6821 = CARTESIAN_POINT ( 'NONE',  ( -32.93157973858376408, 14.54341967768581867, -2.999999999999986677 ) ) ;
#6822 = VERTEX_POINT ( 'NONE', #6251 ) ;
#6823 = DIRECTION ( 'NONE',  ( -0.9147661038495520369, 0.4039838799357109433, 3.987490689252511604E-16 ) ) ;
#6824 = CARTESIAN_POINT ( 'NONE',  ( -4.882243101556620779, -59.05916974321930724, 0.3521297881290503806 ) ) ;
#6825 = DIRECTION ( 'NONE',  ( -0.9793199139485099236, -0.2023178344681531016, -1.787644449902631719E-16 ) ) ;
#6826 = CARTESIAN_POINT ( 'NONE',  ( -14.02739156872318027, -37.17434273187110705, -0.4662714048949997969 ) ) ;
#6827 = CARTESIAN_POINT ( 'NONE',  ( -1.315849457849963988, -65.60036621133420454, 0.8401019477754300135 ) ) ;
#6828 = CARTESIAN_POINT ( 'NONE',  ( 27.88122153832714645, -34.70413869602577961, 3.503763267581128549 ) ) ;
#6829 = EDGE_CURVE ( 'NONE', #4908, #555, #2448, .T. ) ;
#6830 = FACE_OUTER_BOUND ( 'NONE', #5137, .T. ) ;
#6831 = EDGE_CURVE ( 'NONE', #3341, #4778, #3257, .T. ) ;
#6832 = ORIENTED_EDGE ( 'NONE', *, *, #261, .F. ) ;
#6833 = ORIENTED_EDGE ( 'NONE', *, *, #1409, .F. ) ;
#6834 = ORIENTED_EDGE ( 'NONE', *, *, #6680, .T. ) ;
#6835 = CONTEXT_DEPENDENT_SHAPE_REPRESENTATION ( #7026, #7166 ) ;
#6836 = DIRECTION ( 'NONE',  ( 0.3128416502900965290, -0.9445788350777318820, 0.09950339776592408148 ) ) ;
#6837 = ORIENTED_EDGE ( 'NONE', *, *, #1589, .F. ) ;
#6838 = CARTESIAN_POINT ( 'NONE',  ( -35.54168210215662072, 14.82156649444486263, -2.250000000002000178 ) ) ;
#6839 = DIRECTION ( 'NONE',  ( 1.000000000000000000, 0.000000000000000000, 0.000000000000000000 ) ) ;
#6840 = DIRECTION ( 'NONE',  ( -0.9721221936972339606, -0.2344748185227520099, 0.000000000000000000 ) ) ;
#6841 = CARTESIAN_POINT ( 'NONE',  ( -6.626722312431940765, -62.23055248060769884, 1.814117920127710226 ) ) ;
#6842 = ORIENTED_EDGE ( 'NONE', *, *, #5518, .T. ) ;
#6843 = EDGE_CURVE ( 'NONE', #7068, #1236, #2663, .T. ) ;
#6844 = ORIENTED_EDGE ( 'NONE', *, *, #942, .T. ) ;
#6845 = VECTOR ( 'NONE', #7042, 1000.000000000000114 ) ;
#6846 = DIRECTION ( 'NONE',  ( -5.715354789845005112E-18, -9.999836672264339449E-16, 1.000000000000000000 ) ) ;
#6847 = PRESENTATION_STYLE_ASSIGNMENT (( #5808 ) ) ;
#6848 = DIRECTION ( 'NONE',  ( 0.9999836672264332815, -0.005715354789847320975, 0.000000000000000000 ) ) ;
#6849 = CARTESIAN_POINT ( 'NONE',  ( -7.672523287152989369, -8.566351989504937592, -8.673617379884035472E-15 ) ) ;
#6850 = CIRCLE ( 'NONE', #955, 4.000000000000000000 ) ;
#6851 = CARTESIAN_POINT ( 'NONE',  ( -28.26642576027046516, -36.90973657692984489, -3.001000000000038082 ) ) ;
#6852 = CARTESIAN_POINT ( 'NONE',  ( 37.98783301546301061, 6.414454976836671207, -1.055128867088878541 ) ) ;
#6853 = EDGE_CURVE ( 'NONE', #6538, #138, #5687, .T. ) ;
#6854 = VERTEX_POINT ( 'NONE', #6762 ) ;
#6855 = CIRCLE ( 'NONE', #4094, 140.0000000000000284 ) ;
#6856 = CARTESIAN_POINT ( 'NONE',  ( 18.15174781562791395, -39.66224293516708599, 3.307682183023668454 ) ) ;
#6857 = DIRECTION ( 'NONE',  ( -5.715354789860003484E-18, -9.999836672264337477E-16, 1.000000000000000000 ) ) ;
#6858 = DIRECTION ( 'NONE',  ( -0.2344748185227521209, 0.9721221936972339606, 0.000000000000000000 ) ) ;
#6859 = CARTESIAN_POINT ( 'NONE',  ( 6.836834775951150078, -58.56388191083841122, -1.340052733437185895 ) ) ;
#6860 = CARTESIAN_POINT ( 'NONE',  ( 37.86567095459282228, 7.005780695865149177, -1.500000000001998623 ) ) ;
#6861 = EDGE_LOOP ( 'NONE', ( #2634, #6137, #6798, #6718 ) ) ;
#6862 = CARTESIAN_POINT ( 'NONE',  ( -4.803738746926375036, -62.03564609396137541, 2.885421999583970720 ) ) ;
#6863 = ADVANCED_FACE ( 'NONE', ( #3338 ), #4556, .F. ) ;
#6864 = CARTESIAN_POINT ( 'NONE',  ( -28.02385480137100160, 13.25058454003099939, -1.493845543551999944 ) ) ;
#6865 = DIRECTION ( 'NONE',  ( -5.715354789845005112E-18, -9.999836672264339449E-16, 1.000000000000000000 ) ) ;
#6866 = CARTESIAN_POINT ( 'NONE',  ( 3.023925381325990092, -64.82443887782423531, -1.545558412227113765 ) ) ;
#6867 = CARTESIAN_POINT ( 'NONE',  ( 27.40805635163918907, -34.38841731323995532, 3.804002023004813271 ) ) ;
#6868 = CARTESIAN_POINT ( 'NONE',  ( 43.45632180942044442, -94.90042465344848210, -3.001370543551634906 ) ) ;
#6869 = VERTEX_POINT ( 'NONE', #4173 ) ;
#6870 = AXIS2_PLACEMENT_3D ( 'NONE', #3773, #953, #6203 ) ;
#6871 = EDGE_LOOP ( 'NONE', ( #3137, #372, #3910, #4584 ) ) ;
#6872 = VERTEX_POINT ( 'NONE', #6989 ) ;
#6873 = EDGE_LOOP ( 'NONE', ( #2138, #5417, #2364, #2812, #1344, #5072 ) ) ;
#6874 = EDGE_CURVE ( 'NONE', #6757, #6490, #1765, .T. ) ;
#6875 = ADVANCED_FACE ( 'NONE', ( #7439 ), #2880, .F. ) ;
#6876 = CARTESIAN_POINT ( 'NONE',  ( -13.14279338728291080, 13.42477640308646514, 3.000000000000013323 ) ) ;
#6877 = VERTEX_POINT ( 'NONE', #4596 ) ;
#6878 = AXIS2_PLACEMENT_3D ( 'NONE', #7155, #7369, #5735 ) ;
#6879 = CARTESIAN_POINT ( 'NONE',  ( -4.418648243523263019, 30.02574454609010246, 3.000000000000030198 ) ) ;
#6880 = LINE ( 'NONE', #7289, #4255 ) ;
#6881 = DIRECTION ( 'NONE',  ( 0.000000000000000000, -0.000000000000000000, 1.000000000000000000 ) ) ;
#6882 = CARTESIAN_POINT ( 'NONE',  ( -3.551508372363994859, -54.02225908916108210, 1.181396430060940306 ) ) ;
#6883 = ORIENTED_EDGE ( 'NONE', *, *, #1043, .T. ) ;
#6884 = ORIENTED_EDGE ( 'NONE', *, *, #2180, .F. ) ;
#6885 = AXIS2_PLACEMENT_3D ( 'NONE', #7013, #3658, #4187 ) ;
#6886 = AXIS2_PLACEMENT_3D ( 'NONE', #6694, #5007, #3941 ) ;
#6887 = FILL_AREA_STYLE ('',( #1172 ) ) ;
#6888 = ADVANCED_FACE ( 'NONE', ( #6926 ), #5849, .T. ) ;
#6889 = CARTESIAN_POINT ( 'NONE',  ( -22.27644891976294161, 9.837844043328892951, 0.006154456448479242447 ) ) ;
#6890 = VECTOR ( 'NONE', #6682, 1000.000000000000114 ) ;
#6891 = DIRECTION ( 'NONE',  ( 0.8688689365825387201, 0.4950421911735688463, 4.999999999999993486E-16 ) ) ;
#6892 = AXIS2_PLACEMENT_3D ( 'NONE', #1039, #3364, #1115 ) ;
#6893 = CARTESIAN_POINT ( 'NONE',  ( 6.419789085491157898, -62.60659963283899998, -3.157657936188097203 ) ) ;
#6894 = CARTESIAN_POINT ( 'NONE',  ( -16.44258018226587836, 7.261459853215404436, -0.3999035282155121718 ) ) ;
#6895 = CARTESIAN_POINT ( 'NONE',  ( -14.18862021369882775, 3.785219303680396052, 13.68921345764850450 ) ) ;
#6896 =( GEOMETRIC_REPRESENTATION_CONTEXT ( 3 ) GLOBAL_UNCERTAINTY_ASSIGNED_CONTEXT ( ( #2072 ) ) GLOBAL_UNIT_ASSIGNED_CONTEXT ( ( #5276, #367, #4362 ) ) REPRESENTATION_CONTEXT ( 'NONE', 'WORKASPACE' ) );
#6897 = ORIENTED_EDGE ( 'NONE', *, *, #579, .T. ) ;
#6898 = ORIENTED_EDGE ( 'NONE', *, *, #1928, .T. ) ;
#6899 = CIRCLE ( 'NONE', #3641, 3.750000000000000000 ) ;
#6900 = CIRCLE ( 'NONE', #3643, 140.0000000000000000 ) ;
#6901 = VECTOR ( 'NONE', #4406, 1000.000000000000000 ) ;
#6902 = CARTESIAN_POINT ( 'NONE',  ( 18.28020086966458990, -39.58905619933629083, 3.436919340399352318 ) ) ;
#6903 = CARTESIAN_POINT ( 'NONE',  ( -40.65229780501022816, -93.90085982332443848, -9.413166846682193472E-14 ) ) ;
#6904 = AXIS2_PLACEMENT_3D ( 'NONE', #1779, #4074, #463 ) ;
#6905 = DIRECTION ( 'NONE',  ( 0.000000000000000000, -0.7252570966694443788, 0.6884781359858918037 ) ) ;
#6906 = CARTESIAN_POINT ( 'NONE',  ( -3.648210298237669846, -66.52323838441711246, -0.5446899798612400145 ) ) ;
#6907 = DIRECTION ( 'NONE',  ( -0.8039121061460985374, 0.3550279469270785082, -0.4771587602596095712 ) ) ;
#6908 = CIRCLE ( 'NONE', #4633, 0.5000000000000004441 ) ;
#6909 = VERTEX_POINT ( 'NONE', #4092 ) ;
#6910 = CARTESIAN_POINT ( 'NONE',  ( -32.92087242456759100, 14.53869105662955619, 0.006154456448484012937 ) ) ;
#6911 = CARTESIAN_POINT ( 'NONE',  ( 14.63724902514211834, -35.33341991383040437, 3.658178766884810251 ) ) ;
#6912 = CARTESIAN_POINT ( 'NONE',  ( -40.82267254781529431, -94.88271315313488685, -3.000000000000095923 ) ) ;
#6913 = VECTOR ( 'NONE', #6891, 1000.000000000000000 ) ;
#6914 = DIRECTION ( 'NONE',  ( 0.4039838799357096111, 0.9147661038495524810, -1.228182406907795247E-16 ) ) ;
#6915 = CARTESIAN_POINT ( 'NONE',  ( 5.755397240816559901, -61.80640411027656000, 0.6650717595513898628 ) ) ;
#6916 = DIRECTION ( 'NONE',  ( 0.000000000000000000, -1.000000000000000000, -8.673617379884027583E-16 ) ) ;
#6917 = DIRECTION ( 'NONE',  ( -0.9492883822130750993, 0.3144066910790588865, 0.000000000000000000 ) ) ;
#6918 = EDGE_LOOP ( 'NONE', ( #5154, #6106, #842, #3342 ) ) ;
#6919 = EDGE_CURVE ( 'NONE', #5943, #2204, #5876, .T. ) ;
#6920 = ORIENTED_EDGE ( 'NONE', *, *, #910, .T. ) ;
#6921 = VERTEX_POINT ( 'NONE', #3417 ) ;
#6922 = CONTEXT_DEPENDENT_SHAPE_REPRESENTATION ( #6542, #1761 ) ;
#6923 = LINE ( 'NONE', #5193, #4129 ) ;
#6924 = CARTESIAN_POINT ( 'NONE',  ( 5.927764221498110331, -62.35749858221746678, -1.529935281190306862 ) ) ;
#6925 = CARTESIAN_POINT ( 'NONE',  ( 5.766865232587130130, -57.44905037028758699, 0.3380538640060152256 ) ) ;
#6926 = FACE_OUTER_BOUND ( 'NONE', #1644, .T. ) ;
#6927 = CARTESIAN_POINT ( 'NONE',  ( 4.666229687490379696, -57.64092629874981810, -1.544454925248829991 ) ) ;
#6928 = VERTEX_POINT ( 'NONE', #673 ) ;
#6929 = FACE_OUTER_BOUND ( 'NONE', #4734, .T. ) ;
#6930 = DIRECTION ( 'NONE',  ( -5.715354789860003484E-18, -9.999836672264337477E-16, 1.000000000000000000 ) ) ;
#6931 = FACE_OUTER_BOUND ( 'NONE', #1793, .T. ) ;
#6932 = CARTESIAN_POINT ( 'NONE',  ( 43.95483829995806957, -94.87490738911687060, -9.454242944073598665E-14 ) ) ;
#6933 = CARTESIAN_POINT ( 'NONE',  ( -16.40387102536037744, 1.778486824056636939, 3.000000000000001776 ) ) ;
#6934 = ORIENTED_EDGE ( 'NONE', *, *, #4113, .F. ) ;
#6935 = ADVANCED_FACE ( 'NONE', ( #1832 ), #5733, .T. ) ;
#6936 = ADVANCED_FACE ( 'NONE', ( #1203 ), #3912, .T. ) ;
#6937 = ORIENTED_EDGE ( 'NONE', *, *, #5043, .T. ) ;
#6938 = DIRECTION ( 'NONE',  ( -0.3144019573014875113, 0.9492899500389717637, 0.000000000000000000 ) ) ;
#6939 = FACE_OUTER_BOUND ( 'NONE', #6957, .T. ) ;
#6940 = CARTESIAN_POINT ( 'NONE',  ( 104.0973215944787711, -119.5240462704291389, -3.000000000000119904 ) ) ;
#6941 = CARTESIAN_POINT ( 'NONE',  ( -12.80424950550273167, -30.40040925781620373, -3.000000000000031086 ) ) ;
#6942 = VERTEX_POINT ( 'NONE', #2430 ) ;
#6943 = CARTESIAN_POINT ( 'NONE',  ( -5.032169712422947860, -62.11039060171678017, 3.232780297333488040 ) ) ;
#6944 = LINE ( 'NONE', #92, #5351 ) ;
#6945 = CARTESIAN_POINT ( 'NONE',  ( 1.714606436958001585E-17, 2.999951001679301835E-15, -3.000000000000000888 ) ) ;
#6946 = CARTESIAN_POINT ( 'NONE',  ( -9.311346830843410416, -51.41373841511902043, 2.533728595105000370 ) ) ;
#6947 = CARTESIAN_POINT ( 'NONE',  ( 5.113035703684060351, -58.96629286118465529, 0.1341944340671852032 ) ) ;
#6948 = CARTESIAN_POINT ( 'NONE',  ( -5.563801105733269914, -63.69014839564722763, 1.341242183458755344 ) ) ;
#6949 = CARTESIAN_POINT ( 'NONE',  ( -30.62055434958606170, 13.52281233407238403, -8.815182418718723767 ) ) ;
#6950 = VERTEX_POINT ( 'NONE', #1869 ) ;
#6951 = ORIENTED_EDGE ( 'NONE', *, *, #381, .F. ) ;
#6952 = CARTESIAN_POINT ( 'NONE',  ( 7.529070345495034289, 16.11642554373086256, 1.000000000000015987 ) ) ;
#6953 = CARTESIAN_POINT ( 'NONE',  ( -3.427937952159080037, -54.92350006295870202, -2.312565912944844371 ) ) ;
#6954 = CARTESIAN_POINT ( 'NONE',  ( 27.30483167885241969, -34.44723005938377014, -0.06578604103650731449 ) ) ;
#6955 = ORIENTED_EDGE ( 'NONE', *, *, #2970, .F. ) ;
#6956 = ORIENTED_EDGE ( 'NONE', *, *, #858, .T. ) ;
#6957 = EDGE_LOOP ( 'NONE', ( #6023, #6588, #3740, #6340, #6499 ) ) ;
#6958 = CARTESIAN_POINT ( 'NONE',  ( 12.89845119661129758, 18.96985124815245527, -2.671436925771697446 ) ) ;
#6959 = EDGE_CURVE ( 'NONE', #3782, #2276, #6520, .T. ) ;
#6960 = PLANE ( 'NONE',  #889 ) ;
#6961 = FACE_OUTER_BOUND ( 'NONE', #3181, .T. ) ;
#6962 = CARTESIAN_POINT ( 'NONE',  ( 1.785462125252589960, -54.25404267560509908, 2.136629312307830375 ) ) ;
#6963 = SURFACE_STYLE_FILL_AREA ( #3384 ) ;
#6964 = CARTESIAN_POINT ( 'NONE',  ( -4.470547512179178895, -58.04376326654274720, -1.678768375691622960 ) ) ;
#6965 = VECTOR ( 'NONE', #5821, 1000.000000000000000 ) ;
#6966 = EDGE_CURVE ( 'NONE', #4731, #1000, #316, .T. ) ;
#6967 = PLANE ( 'NONE',  #4119 ) ;
#6968 = EDGE_CURVE ( 'NONE', #6686, #6942, #2075, .T. ) ;
#6969 = DIRECTION ( 'NONE',  ( 0.9999836672264332815, -0.005715354789845002517, 0.000000000000000000 ) ) ;
#6970 = DIRECTION ( 'NONE',  ( 0.7411265327553913096, 0.6713653717953970146, 6.755902076156640294E-16 ) ) ;
#6971 = DIRECTION ( 'NONE',  ( 5.715354789860003484E-18, 9.999836672264337477E-16, -1.000000000000000000 ) ) ;
#6972 = AXIS2_PLACEMENT_3D ( 'NONE', #386, #1549, #6231 ) ;
#6973 = ORIENTED_EDGE ( 'NONE', *, *, #3082, .T. ) ;
#6974 = LINE ( 'NONE', #3961, #736 ) ;
#6975 = ADVANCED_FACE ( 'NONE', ( #1434 ), #7196, .F. ) ;
#6976 = AXIS2_PLACEMENT_3D ( 'NONE', #2775, #3309, #378 ) ;
#6977 = DIRECTION ( 'NONE',  ( -5.715354789845005112E-18, -9.999836672264339449E-16, 1.000000000000000000 ) ) ;
#6978 = CARTESIAN_POINT ( 'NONE',  ( -4.716938577623720263, -57.97996379370297149, -0.6608593144672147979 ) ) ;
#6979 = CARTESIAN_POINT ( 'NONE',  ( -5.628700163094269016, -63.23550210468251009, 3.461537593744290042 ) ) ;
#6980 = LINE ( 'NONE', #664, #6274 ) ;
#6981 = B_SPLINE_CURVE_WITH_KNOTS ( 'NONE', 3,
 ( #60, #5149, #6314, #5717, #6791, #7426, #2866, #2268 ),
 .UNSPECIFIED., .F., .F.,
 ( 4, 2, 2, 4 ),
 ( 4.924395521842310123E-19, 0.0003905878508574884894, 0.0007811757017149765451, 0.001562351403429946151 ),
 .UNSPECIFIED. ) ;
#6982 = ORIENTED_EDGE ( 'NONE', *, *, #1180, .F. ) ;
#6983 = EDGE_LOOP ( 'NONE', ( #4054, #363, #3823, #2953 ) ) ;
#6984 = AXIS2_PLACEMENT_3D ( 'NONE', #171, #7125, #4345 ) ;
#6985 = CARTESIAN_POINT ( 'NONE',  ( -12.36403222600316276, 10.92614786255227166, -2.999999999999990230 ) ) ;
#6986 = EDGE_CURVE ( 'NONE', #3009, #1758, #4983, .T. ) ;
#6987 = DIRECTION ( 'NONE',  ( -0.9721221936972339606, -0.2344748185227520376, 0.000000000000000000 ) ) ;
#6988 = CARTESIAN_POINT ( 'NONE',  ( 6.871427970997950219, -62.19563859352643931, -1.162241389626079702 ) ) ;
#6989 = CARTESIAN_POINT ( 'NONE',  ( -14.18459254737392072, -36.69969775685165558, -2.566271404894997499 ) ) ;
#6990 = VERTEX_POINT ( 'NONE', #1477 ) ;
#6991 = ORIENTED_EDGE ( 'NONE', *, *, #77, .F. ) ;
#6992 = VECTOR ( 'NONE', #2748, 1000.000000000000000 ) ;
#6993 = CARTESIAN_POINT ( 'NONE',  ( 39.48483786921892857, -95.33781693134928048, 2.999999999999904521 ) ) ;
#6994 = CARTESIAN_POINT ( 'NONE',  ( -28.22553731214382111, -35.79092421365019305, -3.000000000000036859 ) ) ;
#6995 = FACE_BOUND ( 'NONE', #5234, .T. ) ;
#6996 = DIRECTION ( 'NONE',  ( -0.9858503002877112564, 0.1676281164441980331, 1.619908943762944784E-16 ) ) ;
#6997 = CARTESIAN_POINT ( 'NONE',  ( 2.808545138791364693, -54.80713269388122200, 2.194622045337712102 ) ) ;
#6998 = AXIS2_PLACEMENT_3D ( 'NONE', #866, #7156, #1995 ) ;
#6999 = CARTESIAN_POINT ( 'NONE',  ( 5.178445921634760474, -62.11857673748845343, 0.8408583081513953950 ) ) ;
#7000 = ADVANCED_FACE ( 'NONE', ( #349 ), #4203, .T. ) ;
#7001 = COLOUR_RGB ( '', 0.09019608, 0.27058824, 0.51372549) ;
#7002 = CARTESIAN_POINT ( 'NONE',  ( -4.663084970140659813, -61.97199652813008441, 2.252239320826900482 ) ) ;
#7003 = AXIS2_PLACEMENT_3D ( 'NONE', #6101, #3212, #5532 ) ;
#7004 = CARTESIAN_POINT ( 'NONE',  ( -35.54168210215661361, 14.82156649444488394, -1.500000000001999956 ) ) ;
#7005 = CARTESIAN_POINT ( 'NONE',  ( 2.672475618906553940, -55.25697960364365713, 0.2490731612973094422 ) ) ;
#7006 = CARTESIAN_POINT ( 'NONE',  ( -5.509265921604280081, -56.99747518668161206, -0.3692125993829896702 ) ) ;
#7007 = AXIS2_PLACEMENT_3D ( 'NONE', #6879, #1125, #2807 ) ;
#7008 = VECTOR ( 'NONE', #4806, 1000.000000000000227 ) ;
#7009 = ORIENTED_EDGE ( 'NONE', *, *, #5043, .F. ) ;
#7010 = EDGE_CURVE ( 'NONE', #7434, #7283, #2473, .T. ) ;
#7011 = EDGE_CURVE ( 'NONE', #888, #1198, #169, .T. ) ;
#7012 =( GEOMETRIC_REPRESENTATION_CONTEXT ( 3 ) GLOBAL_UNCERTAINTY_ASSIGNED_CONTEXT ( ( #430 ) ) GLOBAL_UNIT_ASSIGNED_CONTEXT ( ( #5507, #330, #7285 ) ) REPRESENTATION_CONTEXT ( 'NONE', 'WORKASPACE' ) );
#7013 = CARTESIAN_POINT ( 'NONE',  ( 18.04796579205319063, 16.34913706177017190, 3.306154456448485490 ) ) ;
#7014 = AXIS2_PLACEMENT_3D ( 'NONE', #6932, #5249, #2967 ) ;
#7015 = CIRCLE ( 'NONE', #4007, 2.249999999999962252 ) ;
#7016 = FACE_OUTER_BOUND ( 'NONE', #2838, .T. ) ;
#7017 = CARTESIAN_POINT ( 'NONE',  ( 5.447354608442940282, -62.18425133612383604, -1.411124226719259855 ) ) ;
#7018 = FACE_OUTER_BOUND ( 'NONE', #1974, .T. ) ;
#7019 = CARTESIAN_POINT ( 'NONE',  ( -13.19674249314596892, -2.997380612392114951, -3.072755722272031268E-15 ) ) ;
#7020 = ORIENTED_EDGE ( 'NONE', *, *, #4152, .F. ) ;
#7021 = EDGE_LOOP ( 'NONE', ( #1119, #2875, #3833, #7147 ) ) ;
#7022 = EDGE_CURVE ( 'NONE', #6347, #2788, #3045, .T. ) ;
#7023 = EDGE_CURVE ( 'NONE', #2665, #1675, #5052, .T. ) ;
#7024 = ORIENTED_EDGE ( 'NONE', *, *, #5487, .T. ) ;
#7025 = VERTEX_POINT ( 'NONE', #2680 ) ;
#7026 =( REPRESENTATION_RELATIONSHIP ('NONE','NONE', #3195, #3150 ) REPRESENTATION_RELATIONSHIP_WITH_TRANSFORMATION ( #5122 )SHAPE_REPRESENTATION_RELATIONSHIP( ) );
#7027 = CARTESIAN_POINT ( 'NONE',  ( 24.80820526761568345, 22.47304504285837368, -8.815182418718737978 ) ) ;
#7028 = ORIENTED_EDGE ( 'NONE', *, *, #1940, .T. ) ;
#7029 = DIRECTION ( 'NONE',  ( 0.000000000000000000, 0.000000000000000000, -1.000000000000000000 ) ) ;
#7030 = CARTESIAN_POINT ( 'NONE',  ( 6.134453413605339911, -63.99854120705014537, -1.074823505768055742 ) ) ;
#7031 = CARTESIAN_POINT ( 'NONE',  ( 27.74785682929057629, -34.19481438196219614, -0.1328907850162961701 ) ) ;
#7032 = CIRCLE ( 'NONE', #5485, 5.000000000000000000 ) ;
#7033 = EDGE_CURVE ( 'NONE', #4585, #1522, #534, .T. ) ;
#7034 = ORIENTED_EDGE ( 'NONE', *, *, #2598, .T. ) ;
#7035 =( NAMED_UNIT ( * ) PLANE_ANGLE_UNIT ( ) SI_UNIT ( $, .RADIAN. ) );
#7036 = CARTESIAN_POINT ( 'NONE',  ( -45.21893524706405287, -93.36435596057614816, -3.001000000000094925 ) ) ;
#7037 = DIRECTION ( 'NONE',  ( 0.000000000000000000, 0.000000000000000000, -1.000000000000000000 ) ) ;
#7038 = CYLINDRICAL_SURFACE ( 'NONE', #3885, 2.999999999999999556 ) ;
#7039 = CARTESIAN_POINT ( 'NONE',  ( 0.000000000000000000, 0.000000000000000000, 3.000000000000000000 ) ) ;
#7040 = CARTESIAN_POINT ( 'NONE',  ( 3.116905194451685013, -55.41725085606579171, 2.344137946175070653 ) ) ;
#7041 = DIRECTION ( 'NONE',  ( 0.9492899500389725409, 0.3144019573014856794, 0.000000000000000000 ) ) ;
#7042 = DIRECTION ( 'NONE',  ( -0.02358931830619094214, 0.9997217333147505602, 9.995705837626804294E-16 ) ) ;
#7043 = EDGE_CURVE ( 'NONE', #5496, #4908, #4988, .T. ) ;
#7044 = DIRECTION ( 'NONE',  ( 0.1860016876085203719, -0.1636620475539280195, 0.9688230521603200529 ) ) ;
#7045 = CARTESIAN_POINT ( 'NONE',  ( -6.079305786110669629, -62.05959118544440400, 1.459294228111509995 ) ) ;
#7046 = ORIENTED_EDGE ( 'NONE', *, *, #4495, .F. ) ;
#7047 = SHAPE_REPRESENTATION ( 'Return Torsion Spring', ( #751 ), #6896 ) ;
#7048 = CARTESIAN_POINT ( 'NONE',  ( 23.12979183812720407, 24.32586137474685017, -8.815182418718713109 ) ) ;
#7049 = DIRECTION ( 'NONE',  ( -5.715354789851314459E-18, -9.999836672264284229E-16, 1.000000000000000000 ) ) ;
#7050 = DIRECTION ( 'NONE',  ( 0.9123165276958903336, 0.4094857180573137079, 4.146932426562371539E-16 ) ) ;
#7051 = ADVANCED_FACE ( 'NONE', ( #5524, #2607, #6708 ), #3239, .F. ) ;
#7052 = CARTESIAN_POINT ( 'NONE',  ( -5.996378862946620814, -62.15612413928192836, 3.522786485084270058 ) ) ;
#7053 = CARTESIAN_POINT ( 'NONE',  ( 2.671142801832544933, -55.70169962949673703, -1.720663637103989618 ) ) ;
#7054 = CARTESIAN_POINT ( 'NONE',  ( 26.67188031194815068, 24.16129507000589527, -2.993845543551515664 ) ) ;
#7055 = DIRECTION ( 'NONE',  ( -0.5224671166576538850, 0.8526594349512809368, 0.000000000000000000 ) ) ;
#7056 = VERTEX_POINT ( 'NONE', #7231 ) ;
#7057 = ORIENTED_EDGE ( 'NONE', *, *, #3831, .T. ) ;
#7058 = EDGE_LOOP ( 'NONE', ( #22, #3697, #1385, #7066 ) ) ;
#7059 = FACE_OUTER_BOUND ( 'NONE', #1131, .T. ) ;
#7060 = VERTEX_POINT ( 'NONE', #5557 ) ;
#7061 = DIRECTION ( 'NONE',  ( -0.005715354789845003385, -0.9999836672264335036, -2.228438827623913869E-16 ) ) ;
#7062 = ADVANCED_FACE ( 'NONE', ( #3648 ), #4866, .F. ) ;
#7063 = ADVANCED_FACE ( 'NONE', ( #3510 ), #5786, .F. ) ;
#7064 = CARTESIAN_POINT ( 'NONE',  ( 6.272193759149150338, -58.74577472516177323, -1.694429590687548837 ) ) ;
#7065 = DIRECTION ( 'NONE',  ( 5.715354789860003484E-18, 9.999836672264337477E-16, -1.000000000000000000 ) ) ;
#7066 = ORIENTED_EDGE ( 'NONE', *, *, #1040, .F. ) ;
#7067 = VERTEX_POINT ( 'NONE', #5999 ) ;
#7068 = VERTEX_POINT ( 'NONE', #4787 ) ;
#7069 = CARTESIAN_POINT ( 'NONE',  ( -28.68093632328457332, 11.79168739492758711, -1.499999999999988676 ) ) ;
#7070 = CARTESIAN_POINT ( 'NONE',  ( -14.70408710852078116, -35.66654345889202204, -3.000000000000036415 ) ) ;
#7071 = DIRECTION ( 'NONE',  ( -0.9147661038495488173, 0.4039838799357178822, 1.577721810442023611E-30 ) ) ;
#7072 = CARTESIAN_POINT ( 'NONE',  ( 1.159215146223531834, -55.24985087088717250, -0.2200125624336850272 ) ) ;
#7073 = CARTESIAN_POINT ( 'NONE',  ( 14.12411727399747186, 19.86467175049790868, 0.006154456448484880299 ) ) ;
#7074 = CARTESIAN_POINT ( 'NONE',  ( -5.480856739662490540, -62.25220485324549458, 1.560007870815685260 ) ) ;
#7075 = CARTESIAN_POINT ( 'NONE',  ( 5.174390334401523184, -63.14351876211269854, -1.324289845673988442 ) ) ;
#7076 = CARTESIAN_POINT ( 'NONE',  ( -5.671911954242359499, -63.61502870002530585, -0.7222274751851948116 ) ) ;
#7077 = EDGE_LOOP ( 'NONE', ( #625, #1760, #242, #6550 ) ) ;
#7078 = DIRECTION ( 'NONE',  ( 0.8474369140690223290, -0.5308961072311347840, -5.260440335992994916E-16 ) ) ;
#7079 = AXIS2_PLACEMENT_3D ( 'NONE', #5483, #3158, #3193 ) ;
#7080 = CARTESIAN_POINT ( 'NONE',  ( 94.42889356597736139, -103.2882618349535591, -3.000000000000103917 ) ) ;
#7081 = CARTESIAN_POINT ( 'NONE',  ( 18.26921625715436193, -39.59531473433197135, -0.9790311301541629874 ) ) ;
#7082 = DIRECTION ( 'NONE',  ( -0.9721221936972339606, -0.2344748185227520376, 0.000000000000000000 ) ) ;
#7083 = AXIS2_PLACEMENT_3D ( 'NONE', #1517, #7341, #7384 ) ;
#7084 = CARTESIAN_POINT ( 'NONE',  ( -6.199032880790720235, -61.56120177486793210, 3.556545127952429830 ) ) ;
#7085 = LINE ( 'NONE', #874, #1339 ) ;
#7086 = ORIENTED_EDGE ( 'NONE', *, *, #1182, .F. ) ;
#7087 = VERTEX_POINT ( 'NONE', #787 ) ;
#7088 = EDGE_CURVE ( 'NONE', #1354, #5496, #745, .T. ) ;
#7089 = CARTESIAN_POINT ( 'NONE',  ( 10.30762257547189975, -51.58645851951763461, -2.495037190209991707 ) ) ;
#7090 = CARTESIAN_POINT ( 'NONE',  ( 0.000000000000000000, 0.000000000000000000, 3.500000000000000000 ) ) ;
#7091 = CARTESIAN_POINT ( 'NONE',  ( 1.014503381694089823, -65.79094358639915185, 1.195300268011630029 ) ) ;
#7092 = ORIENTED_EDGE ( 'NONE', *, *, #3471, .T. ) ;
#7093 = VERTEX_POINT ( 'NONE', #4295 ) ;
#7094 = EDGE_LOOP ( 'NONE', ( #1981, #6084, #7436, #6690, #4398, #4738, #1440, #6054, #852, #5145, #3554, #1530, #6088, #5237, #6363, #6581, #182, #1352, #1674, #2024, #7128, #2422, #6320, #4031, #4399, #5385, #2700, #4928, #405, #2984 ) ) ;
#7095 = ADVANCED_FACE ( 'NONE', ( #5390 ), #3110, .F. ) ;
#7096 = ADVANCED_FACE ( 'NONE', ( #5750 ), #5221, .F. ) ;
#7097 = DIRECTION ( 'NONE',  ( -0.9147661038495495944, 0.4039838799357160504, 3.987490689252424829E-16 ) ) ;
#7098 = DIRECTION ( 'NONE',  ( 0.1860016876085203719, -0.1636620475539280195, 0.9688230521603200529 ) ) ;
#7099 = CARTESIAN_POINT ( 'NONE',  ( 4.781940407807399929, -62.01839479521094489, -2.202197501157848958 ) ) ;
#7100 = CARTESIAN_POINT ( 'NONE',  ( -5.354034084503060065, -64.02545556441495478, -0.7792797212839647214 ) ) ;
#7101 = ORIENTED_EDGE ( 'NONE', *, *, #6506, .F. ) ;
#7102 = ORIENTED_EDGE ( 'NONE', *, *, #2905, .T. ) ;
#7103 = CIRCLE ( 'NONE', #3857, 1.100000000000000755 ) ;
#7104 = EDGE_CURVE ( 'NONE', #1688, #75, #6944, .T. ) ;
#7105 = DIRECTION ( 'NONE',  ( 0.9999836672264332815, -0.005715354789859936752, 0.000000000000000000 ) ) ;
#7106 = CARTESIAN_POINT ( 'NONE',  ( -2.909477865675369923, -55.29415281518058833, 1.990524098341705406 ) ) ;
#7107 = CARTESIAN_POINT ( 'NONE',  ( 9.998427761233271482, -32.39925913208585939, -3.252606517456513302E-14 ) ) ;
#7108 = AXIS2_PLACEMENT_3D ( 'NONE', #6122, #3119, #2601 ) ;
#7109 = VECTOR ( 'NONE', #4443, 999.9999999999998863 ) ;
#7110 = LINE ( 'NONE', #1293, #6965 ) ;
#7111 = CARTESIAN_POINT ( 'NONE',  ( 0.8643374975182065434, -66.22190918914451174, -1.009590967482013601 ) ) ;
#7112 = EDGE_LOOP ( 'NONE', ( #5794, #5723 ) ) ;
#7113 = AXIS2_PLACEMENT_3D ( 'NONE', #5018, #4533, #2781 ) ;
#7114 = CARTESIAN_POINT ( 'NONE',  ( 14.12411727399747186, 19.86467175049790868, 0.006154456448484880299 ) ) ;
#7115 = AXIS2_PLACEMENT_3D ( 'NONE', #3034, #296, #5353 ) ;
#7116 = CIRCLE ( 'NONE', #7360, 0.7499999999999896749 ) ;
#7117 = PLANE ( 'NONE',  #7108 ) ;
#7118 = CYLINDRICAL_SURFACE ( 'NONE', #6083, 140.0000000000000284 ) ;
#7119 = CARTESIAN_POINT ( 'NONE',  ( 18.49916120972751088, -39.46430250869198630, -1.000000000000039524 ) ) ;
#7120 = VECTOR ( 'NONE', #6640, 1000.000000000000114 ) ;
#7121 = B_SPLINE_CURVE_WITH_KNOTS ( 'NONE', 3,
 ( #2188, #1598, #3887, #1034 ),
 .UNSPECIFIED., .F., .F.,
 ( 4, 4 ),
 ( 0.000000000000000000, 1.000000000000000000 ),
 .UNSPECIFIED. ) ;
#7122 = CARTESIAN_POINT ( 'NONE',  ( -3.569041007005829602, -65.81017109676685095, 3.284668648760890264 ) ) ;
#7123 = VECTOR ( 'NONE', #4247, 1000.000000000000000 ) ;
#7124 = CARTESIAN_POINT ( 'NONE',  ( -5.957512881900739465, -64.40555820178136059, 2.727170671215090270 ) ) ;
#7125 = DIRECTION ( 'NONE',  ( -5.715354789860004255E-18, -9.999836672264337477E-16, 1.000000000000000000 ) ) ;
#7126 = ORIENTED_EDGE ( 'NONE', *, *, #4905, .T. ) ;
#7127 = ORIENTED_EDGE ( 'NONE', *, *, #1546, .T. ) ;
#7128 = ORIENTED_EDGE ( 'NONE', *, *, #526, .T. ) ;
#7129 = VECTOR ( 'NONE', #7194, 1000.000000000000000 ) ;
#7130 = CIRCLE ( 'NONE', #24, 1.000000000000000000 ) ;
#7131 = CARTESIAN_POINT ( 'NONE',  ( -35.54168210215662072, 14.82156649444486263, -2.250000000002000178 ) ) ;
#7132 = AXIS2_PLACEMENT_3D ( 'NONE', #4594, #2248, #524 ) ;
#7133 = CARTESIAN_POINT ( 'NONE',  ( 12.15447797363371052, 11.01039466689934798, -3.299999999999988720 ) ) ;
#7134 = CARTESIAN_POINT ( 'NONE',  ( 4.697834216849050115, -63.19072998194386059, -1.190263883463073880 ) ) ;
#7135 = EDGE_CURVE ( 'NONE', #4165, #2064, #7375, .T. ) ;
#7136 = CARTESIAN_POINT ( 'NONE',  ( 6.002340677743171149, -62.35123097424496308, 0.5688650469685809785 ) ) ;
#7137 = VECTOR ( 'NONE', #720, 1000.000000000000114 ) ;
#7138 = EDGE_LOOP ( 'NONE', ( #1154, #900, #6034, #1078 ) ) ;
#7139 = EDGE_LOOP ( 'NONE', ( #7086, #4642, #460, #3469 ) ) ;
#7140 = LINE ( 'NONE', #2510, #7123 ) ;
#7141 = LINE ( 'NONE', #3103, #660 ) ;
#7142 = CIRCLE ( 'NONE', #3538, 5.000000000000000000 ) ;
#7143 = DIRECTION ( 'NONE',  ( -5.715354789845005112E-18, -9.999836672264339449E-16, 1.000000000000000000 ) ) ;
#7144 = CARTESIAN_POINT ( 'NONE',  ( 6.265638173095489982, -61.94185186372677521, 0.5461908750427398873 ) ) ;
#7145 = ADVANCED_FACE ( 'NONE', ( #613 ), #4620, .F. ) ;
#7146 = ORIENTED_EDGE ( 'NONE', *, *, #1539, .F. ) ;
#7147 = ORIENTED_EDGE ( 'NONE', *, *, #112, .T. ) ;
#7148 = CARTESIAN_POINT ( 'NONE',  ( -105.7473861751082040, -118.0666774205683822, 3.999999999999881428 ) ) ;
#7149 = CARTESIAN_POINT ( 'NONE',  ( 4.689255334142830023, -62.66924379293478609, -1.721810340931042793 ) ) ;
#7150 = FACE_OUTER_BOUND ( 'NONE', #4093, .T. ) ;
#7151 = DIRECTION ( 'NONE',  ( 0.3144019573014849023, -0.9492899500389727629, 0.000000000000000000 ) ) ;
#7152 = EDGE_CURVE ( 'NONE', #1826, #4852, #1374, .T. ) ;
#7153 = CARTESIAN_POINT ( 'NONE',  ( 2.694291810223862882, -55.26708005044292094, -1.848825772310153104 ) ) ;
#7154 = ORIENTED_EDGE ( 'NONE', *, *, #1362, .F. ) ;
#7155 = CARTESIAN_POINT ( 'NONE',  ( 22.42915535073480982, 21.39736943723329432, -1.493845543551513444 ) ) ;
#7156 = DIRECTION ( 'NONE',  ( 2.857391495672265093E-16, 4.793132013414519254E-17, 1.000000000000000000 ) ) ;
#7157 = DIRECTION ( 'NONE',  ( 0.9999836672264331705, -0.005715354789860049509, 0.000000000000000000 ) ) ;
#7158 = DIRECTION ( 'NONE',  ( 0.8688689365825388311, 0.4950421911735690128, -8.411011176753749182E-16 ) ) ;
#7159 = CARTESIAN_POINT ( 'NONE',  ( -6.308476396955129850, -59.14191327212131455, -0.5142043607924547954 ) ) ;
#7160 = CARTESIAN_POINT ( 'NONE',  ( -1.318626809553760104, -67.28799943462540512, -1.163043645407473958 ) ) ;
#7161 = DIRECTION ( 'NONE',  ( 0.4039838799357093335, 0.9147661038495527031, 1.550530988647994607E-16 ) ) ;
#7162 = ORIENTED_EDGE ( 'NONE', *, *, #5139, .F. ) ;
#7163 = VERTEX_POINT ( 'NONE', #5261 ) ;
#7164 = ORIENTED_EDGE ( 'NONE', *, *, #4334, .F. ) ;
#7165 = ORIENTED_EDGE ( 'NONE', *, *, #4355, .F. ) ;
#7166 = PRODUCT_DEFINITION_SHAPE ( 'NONE', 'NONE',  #7445 ) ;
#7167 = DIRECTION ( 'NONE',  ( 2.290931512739800066E-16, 1.403768413105889815E-16, 1.000000000000000000 ) ) ;
#7168 = DIRECTION ( 'NONE',  ( 5.715354789845005112E-18, 9.999836672264339449E-16, -1.000000000000000000 ) ) ;
#7169 = CARTESIAN_POINT ( 'NONE',  ( 3.016248221826935083, -64.97666327952782694, -3.135076956698916728 ) ) ;
#7170 = DIRECTION ( 'NONE',  ( 5.715354789845005112E-18, 9.999836672264339449E-16, -1.000000000000000000 ) ) ;
#7171 = CARTESIAN_POINT ( 'NONE',  ( -1.956775878777010869, -54.45555501790917674, -0.1654709460969512602 ) ) ;
#7172 = VERTEX_POINT ( 'NONE', #2352 ) ;
#7173 = ORIENTED_EDGE ( 'NONE', *, *, #3346, .T. ) ;
#7174 = ORIENTED_EDGE ( 'NONE', *, *, #6114, .T. ) ;
#7175 = BREP_WITH_VOIDS ( 'NONE', #5921, ( #6814, #925 ) );
#7176 = APPLICATION_PROTOCOL_DEFINITION ( 'draft international standard', 'automotive_design', 1998, #4578 ) ;
#7177 = DIRECTION ( 'NONE',  ( -5.715354789845005112E-18, -9.999836672264339449E-16, 1.000000000000000000 ) ) ;
#7178 = LINE ( 'NONE', #812, #4517 ) ;
#7179 = CARTESIAN_POINT ( 'NONE',  ( -15.52817266570582611, -38.02681526409561741, -3.000000000000039080 ) ) ;
#7180 = CARTESIAN_POINT ( 'NONE',  ( 3.660823140336725068, -65.74644859602665292, -1.309095517728299907 ) ) ;
#7181 = VERTEX_POINT ( 'NONE', #4217 ) ;
#7182 = VERTEX_POINT ( 'NONE', #5428 ) ;
#7183 = EDGE_CURVE ( 'NONE', #4278, #1742, #2169, .T. ) ;
#7184 = CARTESIAN_POINT ( 'NONE',  ( -28.98392423323678813, 11.10561281703983738, -1.499999999999988676 ) ) ;
#7185 = CARTESIAN_POINT ( 'NONE',  ( 5.164426235684419275, -63.32698789961681030, 0.7537993011490951023 ) ) ;
#7186 = ORIENTED_EDGE ( 'NONE', *, *, #104, .T. ) ;
#7187 = CARTESIAN_POINT ( 'NONE',  ( 1.714606436953501688E-17, 2.999951001679301835E-15, 0.000000000000000000 ) ) ;
#7188 = CARTESIAN_POINT ( 'NONE',  ( 5.766935121390225127, -60.94769942240537119, -1.455549280073787921 ) ) ;
#7189 = ORIENTED_EDGE ( 'NONE', *, *, #198, .F. ) ;
#7190 = EDGE_CURVE ( 'NONE', #7181, #4852, #3997, .T. ) ;
#7191 = EDGE_CURVE ( 'NONE', #5220, #815, #422, .T. ) ;
#7192 = DIRECTION ( 'NONE',  ( 0.3213584079436493934, -0.3547505615521249767, 0.8779981849197495691 ) ) ;
#7193 = DIRECTION ( 'NONE',  ( -5.715354789860003484E-18, -9.999836672264337477E-16, 1.000000000000000000 ) ) ;
#7194 = DIRECTION ( 'NONE',  ( -5.715354789860003484E-18, -9.999836672264337477E-16, 1.000000000000000000 ) ) ;
#7195 = CARTESIAN_POINT ( 'NONE',  ( -14.04303360023105895, -37.12711394412414734, 0.03124720627272013079 ) ) ;
#7196 = PLANE ( 'NONE',  #1737 ) ;
#7197 = CARTESIAN_POINT ( 'NONE',  ( 6.144163068047750365, -64.45449589790229084, 2.063594979539779661 ) ) ;
#7198 = DIRECTION ( 'NONE',  ( -5.715354789845005112E-18, -9.999836672264339449E-16, 1.000000000000000000 ) ) ;
#7199 = CIRCLE ( 'NONE', #951, 5.000000000000000000 ) ;
#7200 = ORIENTED_EDGE ( 'NONE', *, *, #1780, .T. ) ;
#7201 = ORIENTED_EDGE ( 'NONE', *, *, #6733, .T. ) ;
#7202 = ADVANCED_FACE ( 'NONE', ( #1578 ), #4483, .F. ) ;
#7203 = CARTESIAN_POINT ( 'NONE',  ( 14.38741851828413942, 8.077882666870960904, 8.159979933984663174E-15 ) ) ;
#7204 = AXIS2_PLACEMENT_3D ( 'NONE', #3383, #5698, #535 ) ;
#7205 = CARTESIAN_POINT ( 'NONE',  ( 8.042591699913112180, 16.36558300704127689, 1.647987302177966740E-14 ) ) ;
#7206 = CARTESIAN_POINT ( 'NONE',  ( -1.607783425601855054, -65.25734987882880489, 1.942476202525789342 ) ) ;
#7207 = CARTESIAN_POINT ( 'NONE',  ( 41.70778007397900211, -94.98992620957551480, -9.454242944073598665E-14 ) ) ;
#7208 = CARTESIAN_POINT ( 'NONE',  ( -3.636793936007903572, -65.52149246903836399, 1.198211322333656348 ) ) ;
#7209 = ORIENTED_EDGE ( 'NONE', *, *, #1448, .T. ) ;
#7210 = ORIENTED_EDGE ( 'NONE', *, *, #5562, .T. ) ;
#7211 = VERTEX_POINT ( 'NONE', #3713 ) ;
#7212 = AXIS2_PLACEMENT_3D ( 'NONE', #3952, #6261, #7414 ) ;
#7213 = SHAPE_DEFINITION_REPRESENTATION ( #6568, #7047 ) ;
#7214 = CARTESIAN_POINT ( 'NONE',  ( -20.16480223318149356, 14.61937842657788167, 0.006154456448479242447 ) ) ;
#7215 = DIRECTION ( 'NONE',  ( 0.3128463504745289669, 0.9445772445362837777, 0.09950371902099817978 ) ) ;
#7216 = VECTOR ( 'NONE', #5722, 999.9999999999998863 ) ;
#7217 = CARTESIAN_POINT ( 'NONE',  ( 41.70778007397900211, -94.98992620957551480, -9.475926987523308753E-14 ) ) ;
#7218 = CARTESIAN_POINT ( 'NONE',  ( 2.241808083868705115, -67.04438815209937275, -1.340794555410016020 ) ) ;
#7219 = EDGE_LOOP ( 'NONE', ( #5841, #5199, #5904, #2477, #6934, #6833, #5321, #2585, #2913, #6884, #1107, #1584, #3916, #5669, #6800, #814, #4689, #6212, #2952, #2543, #6146, #5118, #4574, #1871, #5793, #6270, #1459, #1649, #3019, #2552 ) ) ;
#7220 = ORIENTED_EDGE ( 'NONE', *, *, #4353, .T. ) ;
#7221 = ORIENTED_EDGE ( 'NONE', *, *, #4240, .F. ) ;
#7222 = VECTOR ( 'NONE', #4053, 1000.000000000000227 ) ;
#7223 = CARTESIAN_POINT ( 'NONE',  ( -9.311346830843410416, -51.41373841511902043, 2.533728595105000370 ) ) ;
#7224 = CARTESIAN_POINT ( 'NONE',  ( 6.265638173095489982, -61.94185186372677521, 0.5461908750427398873 ) ) ;
#7225 = CARTESIAN_POINT ( 'NONE',  ( -40.82267254781525168, -94.88271315313488685, -3.000000000000095923 ) ) ;
#7226 = VECTOR ( 'NONE', #950, 1000.000000000000114 ) ;
#7227 = EDGE_CURVE ( 'NONE', #1198, #6491, #7261, .T. ) ;
#7228 = ORIENTED_EDGE ( 'NONE', *, *, #5854, .T. ) ;
#7229 = LINE ( 'NONE', #6224, #3891 ) ;
#7230 = DIRECTION ( 'NONE',  ( 0.9993328523369457983, -0.03652191451860404420, -3.080977621017558246E-17 ) ) ;
#7231 = CARTESIAN_POINT ( 'NONE',  ( -3.749938752099124972, 0.02143258046197547145, 4.592425496802572929E-31 ) ) ;
#7232 = CARTESIAN_POINT ( 'NONE',  ( 7.003919171491410189, -62.62977488282763261, 1.976316849587809843 ) ) ;
#7233 = DIRECTION ( 'NONE',  ( 5.715354789845005112E-18, 9.999836672264339449E-16, -1.000000000000000000 ) ) ;
#7234 = ADVANCED_FACE ( 'NONE', ( #2101 ), #1542, .F. ) ;
#7235 = AXIS2_PLACEMENT_3D ( 'NONE', #1645, #4869, #6039 ) ;
#7236 = AXIS2_PLACEMENT_3D ( 'NONE', #5435, #5396, #5973 ) ;
#7237 = ORIENTED_EDGE ( 'NONE', *, *, #2334, .T. ) ;
#7238 = AXIS2_PLACEMENT_3D ( 'NONE', #4476, #1647, #5619 ) ;
#7239 = CARTESIAN_POINT ( 'NONE',  ( 15.39542127499540136, -35.83857563806657964, -3.556183125752454544E-14 ) ) ;
#7240 = DIRECTION ( 'NONE',  ( 0.3963837160139272453, 0.9180849359830441925, 9.203354146796070219E-16 ) ) ;
#7241 = VECTOR ( 'NONE', #5343, 1000.000000000000000 ) ;
#7242 = DIRECTION ( 'NONE',  ( -0.8043765792067081311, 0.5941197849118596830, 5.895127837531212072E-16 ) ) ;
#7243 = CARTESIAN_POINT ( 'NONE',  ( -4.663084970140659813, -61.97199652813008441, 2.252239320826900482 ) ) ;
#7244 = CARTESIAN_POINT ( 'NONE',  ( -3.749938752099124972, 0.02143258046192221891, 0.000000000000000000 ) ) ;
#7245 = EDGE_CURVE ( 'NONE', #6077, #1508, #522, .T. ) ;
#7246 = CARTESIAN_POINT ( 'NONE',  ( 1.018343067164889204, -66.66658444643495329, 0.9358771171724069582 ) ) ;
#7247 = EDGE_CURVE ( 'NONE', #6757, #2618, #1360, .T. ) ;
#7248 = ORIENTED_EDGE ( 'NONE', *, *, #1200, .F. ) ;
#7249 = CIRCLE ( 'NONE', #5946, 0.7500000000000003331 ) ;
#7250 = VERTEX_POINT ( 'NONE', #5012 ) ;
#7251 = ORIENTED_EDGE ( 'NONE', *, *, #7152, .T. ) ;
#7252 = AXIS2_PLACEMENT_3D ( 'NONE', #589, #3413, #2915 ) ;
#7253 = CIRCLE ( 'NONE', #2205, 2.999999999999999556 ) ;
#7254 = DIRECTION ( 'NONE',  ( 1.265976809860859428E-17, 1.999959554497627681E-15, -1.000000000000000000 ) ) ;
#7255 = CARTESIAN_POINT ( 'NONE',  ( 3.749938752099124972, -0.02143258046197501002, 0.000000000000000000 ) ) ;
#7256 = CARTESIAN_POINT ( 'NONE',  ( 15.39900769062488806, 3.181283097128406290, -2.999999999999997335 ) ) ;
#7257 = CARTESIAN_POINT ( 'NONE',  ( 43.95774332523846795, -95.00278575785266355, -9.454242944073598665E-14 ) ) ;
#7258 = CARTESIAN_POINT ( 'NONE',  ( 5.619938529503549773, -63.59344562873818774, 0.6343307546824898946 ) ) ;
#7259 = CIRCLE ( 'NONE', #2690, 0.4999999999999995559 ) ;
#7260 = CIRCLE ( 'NONE', #7238, 0.7499999999999872324 ) ;
#7261 = LINE ( 'NONE', #375, #6302 ) ;
#7262 = CARTESIAN_POINT ( 'NONE',  ( 1.402950248545461909, -54.15620739517822813, 0.01614447287717020105 ) ) ;
#7263 = CONICAL_SURFACE ( 'NONE', #4641, 0.7499999999999872324, 1.029744258676647872 ) ;
#7264 = DIRECTION ( 'NONE',  ( -0.9793199139485099236, -0.2023178344681531016, -1.787644449902631719E-16 ) ) ;
#7265 = DIRECTION ( 'NONE',  ( 5.715354789845005112E-18, 9.999836672264339449E-16, -1.000000000000000000 ) ) ;
#7266 = VERTEX_POINT ( 'NONE', #7184 ) ;
#7267 = FACE_OUTER_BOUND ( 'NONE', #809, .T. ) ;
#7268 = DIRECTION ( 'NONE',  ( -0.6713653717953991240, 0.7411265327553895332, 8.112475779533124710E-16 ) ) ;
#7269 = CARTESIAN_POINT ( 'NONE',  ( 6.577191010720946807, -62.60348822714410488, -2.056697675161959893 ) ) ;
#7270 = CARTESIAN_POINT ( 'NONE',  ( 2.241808083868705115, -67.04438815209937275, -1.340794555410016020 ) ) ;
#7271 = CARTESIAN_POINT ( 'NONE',  ( 0.000000000000000000, 0.000000000000000000, 0.000000000000000000 ) ) ;
#7272 = VERTEX_POINT ( 'NONE', #3826 ) ;
#7273 = DIRECTION ( 'NONE',  ( -5.715354789845005112E-18, -9.999836672264339449E-16, 1.000000000000000000 ) ) ;
#7274 = ADVANCED_FACE ( 'NONE', ( #6619 ), #2667, .T. ) ;
#7275 = CARTESIAN_POINT ( 'NONE',  ( -105.7473861751082040, -118.0666774205683822, -1.186117176699141851E-13 ) ) ;
#7276 = DIRECTION ( 'NONE',  ( -0.9999836672264333925, 0.005715354789844388425, 0.000000000000000000 ) ) ;
#7277 = CARTESIAN_POINT ( 'NONE',  ( 4.837585924071849952, -61.97584320105620748, 1.412225657785534327 ) ) ;
#7278 = CARTESIAN_POINT ( 'NONE',  ( 27.65533861039806496, -36.12687000486608468, 2.999999999999964029 ) ) ;
#7279 = CARTESIAN_POINT ( 'NONE',  ( -5.060928412568097556, -56.78184410889874556, -0.3751579969454835739 ) ) ;
#7280 = EDGE_LOOP ( 'NONE', ( #563, #2275, #5171, #4196 ) ) ;
#7281 = EDGE_LOOP ( 'NONE', ( #1367, #3807, #6321, #1080, #5616, #6055 ) ) ;
#7282 = ORIENTED_EDGE ( 'NONE', *, *, #6655, .T. ) ;
#7283 = VERTEX_POINT ( 'NONE', #3262 ) ;
#7284 = EDGE_CURVE ( 'NONE', #2912, #553, #5582, .T. ) ;
#7285 =( NAMED_UNIT ( * ) SI_UNIT ( $, .STERADIAN. ) SOLID_ANGLE_UNIT ( ) );
#7286 = EDGE_CURVE ( 'NONE', #2328, #210, #5700, .T. ) ;
#7287 = CARTESIAN_POINT ( 'NONE',  ( -20.16480223318149356, 14.61937842657788345, -2.993845543551524990 ) ) ;
#7288 = DIRECTION ( 'NONE',  ( -0.2467992669038191755, 0.02032136184815236737, 0.9688535307818070264 ) ) ;
#7289 = CARTESIAN_POINT ( 'NONE',  ( 12.15447797363371052, 11.01039466689934443, 1.127570259384924611E-14 ) ) ;
#7290 = CARTESIAN_POINT ( 'NONE',  ( -7.175161506198990402, -58.91160695923000645, -1.204451995733903935 ) ) ;
#7291 = ORIENTED_EDGE ( 'NONE', *, *, #4197, .T. ) ;
#7292 = VERTEX_POINT ( 'NONE', #2018 ) ;
#7293 = LINE ( 'NONE', #1651, #4964 ) ;
#7294 = DIRECTION ( 'NONE',  ( 5.715354789845005112E-18, 9.999836672264339449E-16, -1.000000000000000000 ) ) ;
#7295 = EDGE_CURVE ( 'NONE', #2243, #936, #5820, .T. ) ;
#7296 = CARTESIAN_POINT ( 'NONE',  ( -1.592557218785495055, -66.68601476236933934, 1.076257986235874764 ) ) ;
#7297 = ORIENTED_EDGE ( 'NONE', *, *, #6919, .T. ) ;
#7298 = DIRECTION ( 'NONE',  ( 0.6713653717953966815, -0.7411265327553919757, -7.372773368101216216E-16 ) ) ;
#7299 = LINE ( 'NONE', #3913, #3240 ) ;
#7300 = ORIENTED_EDGE ( 'NONE', *, *, #7416, .T. ) ;
#7301 = ADVANCED_FACE ( 'NONE', ( #337 ), #3753, .T. ) ;
#7302 = CARTESIAN_POINT ( 'NONE',  ( 18.27066553070502408, -39.59448900386337300, 3.979556571570188162 ) ) ;
#7303 = DIRECTION ( 'NONE',  ( -5.715354789845005112E-18, -9.999836672264339449E-16, 1.000000000000000000 ) ) ;
#7304 = CARTESIAN_POINT ( 'NONE',  ( 24.99346688245966419, 26.01411140189437532, -2.993845543551503674 ) ) ;
#7305 = CARTESIAN_POINT ( 'NONE',  ( -3.328771606340945155, -66.98264282425255089, -1.647280098378362867 ) ) ;
#7306 = DIRECTION ( 'NONE',  ( -0.9147661038495519259, 0.4039838799357108878, 4.130293990420968897E-16 ) ) ;
#7307 = ORIENTED_EDGE ( 'NONE', *, *, #6164, .F. ) ;
#7308 = CARTESIAN_POINT ( 'NONE',  ( 12.40979888490706706, -30.61452125107580713, -3.035766082959412415E-14 ) ) ;
#7309 = CARTESIAN_POINT ( 'NONE',  ( 2.467202665543605011, -65.15865635802147438, 2.695445654378740397 ) ) ;
#7310 = DIRECTION ( 'NONE',  ( 0.9123165276958903336, 0.4094857180573137079, 4.146932426562371539E-16 ) ) ;
#7311 = DIRECTION ( 'NONE',  ( 0.9999836672264332815, -0.005715354789845002517, 0.000000000000000000 ) ) ;
#7312 = CARTESIAN_POINT ( 'NONE',  ( 4.653184118170510253, -62.00177009570858644, -2.783824188434504521 ) ) ;
#7313 = CARTESIAN_POINT ( 'NONE',  ( 27.34784330342383640, -35.00115915984075343, 3.973470358432956040 ) ) ;
#7314 = DIRECTION ( 'NONE',  ( -3.347047707994206215E-17, -9.998250342643943298E-16, 1.000000000000000000 ) ) ;
#7315 = EDGE_LOOP ( 'NONE', ( #1507, #1784, #5724, #6246, #1483, #1699 ) ) ;
#7316 = EDGE_CURVE ( 'NONE', #212, #5062, #5334, .T. ) ;
#7317 = VERTEX_POINT ( 'NONE', #3306 ) ;
#7318 = VERTEX_POINT ( 'NONE', #5046 ) ;
#7319 = AXIS2_PLACEMENT_3D ( 'NONE', #4870, #308, #3229 ) ;
#7320 = CARTESIAN_POINT ( 'NONE',  ( -11.31173072208887831, -97.70380408000731620, -9.757819552369539906E-14 ) ) ;
#7321 = ORIENTED_EDGE ( 'NONE', *, *, #3659, .T. ) ;
#7322 = DIRECTION ( 'NONE',  ( 0.3144066910790611624, 0.9492883822130743221, 0.000000000000000000 ) ) ;
#7323 = CARTESIAN_POINT ( 'NONE',  ( 26.87807528571524074, -34.69037653529182563, -3.447762908503904100E-14 ) ) ;
#7324 = DIRECTION ( 'NONE',  ( 5.715354789845005112E-18, 9.999836672264339449E-16, -1.000000000000000000 ) ) ;
#7325 = CARTESIAN_POINT ( 'NONE',  ( 6.472013764049630247, -56.98767972836586182, 1.711274884184114775 ) ) ;
#7326 = AXIS2_PLACEMENT_3D ( 'NONE', #6707, #3803, #4385 ) ;
#7327 = EDGE_CURVE ( 'NONE', #6322, #2009, #939, .T. ) ;
#7328 = EDGE_CURVE ( 'NONE', #4770, #1906, #4938, .T. ) ;
#7329 = DIRECTION ( 'NONE',  ( -5.715354789845005112E-18, -9.999836672264339449E-16, 1.000000000000000000 ) ) ;
#7330 = DIRECTION ( 'NONE',  ( -0.2163384215910431896, -0.07165063022625259292, 0.9736857165079894072 ) ) ;
#7331 = CARTESIAN_POINT ( 'NONE',  ( 3.403992074353090036, -54.97443010399496899, 2.224669212202579960 ) ) ;
#7332 = TOROIDAL_SURFACE ( 'NONE', #3840, 1.500000000000000000, 1.000000000000000000 ) ;
#7333 = MANIFOLD_SOLID_BREP ( 'NONE', #2056 ) ;
#7334 = CARTESIAN_POINT ( 'NONE',  ( 39.97800414936823188, -95.26063634933134949, 2.999999999999904965 ) ) ;
#7335 = LINE ( 'NONE', #6119, #2524 ) ;
#7336 = ADVANCED_FACE ( 'NONE', ( #35 ), #3226, .F. ) ;
#7337 = AXIS2_PLACEMENT_3D ( 'NONE', #4193, #6386, #5838 ) ;
#7338 = EDGE_LOOP ( 'NONE', ( #5990, #2054, #7210, #4698 ) ) ;
#7339 = FACE_OUTER_BOUND ( 'NONE', #6861, .T. ) ;
#7340 = CARTESIAN_POINT ( 'NONE',  ( -19.94212619460463287, -40.63668738334721553, -3.001000000000041634 ) ) ;
#7341 = DIRECTION ( 'NONE',  ( 5.715354789845005112E-18, 9.999836672264339449E-16, -1.000000000000000000 ) ) ;
#7342 = CARTESIAN_POINT ( 'NONE',  ( 1.647567807763375081, -53.54661630431167652, -1.692287459705078101 ) ) ;
#7343 = DIRECTION ( 'NONE',  ( 0.6713653717953970146, -0.7411265327553913096, -7.372773368101209313E-16 ) ) ;
#7344 = ORIENTED_EDGE ( 'NONE', *, *, #5477, .F. ) ;
#7345 = DIRECTION ( 'NONE',  ( -0.5224671166576538850, 0.8526594349512809368, 0.000000000000000000 ) ) ;
#7346 = CARTESIAN_POINT ( 'NONE',  ( 4.653184118170510253, -62.00177009570858644, -2.783824188434504521 ) ) ;
#7347 = DIRECTION ( 'NONE',  ( 9.251858538542970644E-15, 2.775557561562891351E-14, 1.000000000000000000 ) ) ;
#7348 = DIRECTION ( 'NONE',  ( -0.3144019573014849023, 0.9492899500389726519, 0.000000000000000000 ) ) ;
#7349 = AXIS2_PLACEMENT_3D ( 'NONE', #4382, #5437, #6006 ) ;
#7350 = CARTESIAN_POINT ( 'NONE',  ( 2.818173014649640429, -55.92969527921476924, 1.989760685886134972 ) ) ;
#7351 = CIRCLE ( 'NONE', #2177, 0.5000000000000004441 ) ;
#7352 = CARTESIAN_POINT ( 'NONE',  ( 27.21771279145922406, -34.49686645803022600, 3.307326028875293478 ) ) ;
#7353 = CARTESIAN_POINT ( 'NONE',  ( -5.984900349171567768, -62.40475500745689175, -0.6898787680826136137 ) ) ;
#7354 = ORIENTED_EDGE ( 'NONE', *, *, #6628, .T. ) ;
#7355 = ORIENTED_EDGE ( 'NONE', *, *, #1427, .F. ) ;
#7356 = ORIENTED_EDGE ( 'NONE', *, *, #6778, .F. ) ;
#7357 = AXIS2_PLACEMENT_3D ( 'NONE', #4150, #7041, #6938 ) ;
#7358 = AXIS2_PLACEMENT_3D ( 'NONE', #2368, #3949, #597 ) ;
#7359 = CARTESIAN_POINT ( 'NONE',  ( 15.82006518139331774, 14.33094549030129983, -2.230393353321895145 ) ) ;
#7360 = AXIS2_PLACEMENT_3D ( 'NONE', #5694, #1136, #2367 ) ;
#7361 = EDGE_CURVE ( 'NONE', #3666, #3563, #7116, .T. ) ;
#7362 = CARTESIAN_POINT ( 'NONE',  ( -28.26642576027046516, -36.90973657692984489, -3.001000000000038082 ) ) ;
#7363 = DIRECTION ( 'NONE',  ( -0.6713653717954000122, 0.7411265327553888671, 8.673617379884183383E-16 ) ) ;
#7364 = CARTESIAN_POINT ( 'NONE',  ( 5.975049724055580214, -64.37929422792591083, -2.133092136665421190 ) ) ;
#7365 = VECTOR ( 'NONE', #1201, 1000.000000000000227 ) ;
#7366 = VECTOR ( 'NONE', #6836, 1000.000000000000114 ) ;
#7367 = ORIENTED_EDGE ( 'NONE', *, *, #2113, .T. ) ;
#7368 = AXIS2_PLACEMENT_3D ( 'NONE', #1455, #188, #6579 ) ;
#7369 = DIRECTION ( 'NONE',  ( 0.7411265327553895332, 0.6713653717953992350, 6.755902076156661002E-16 ) ) ;
#7370 = SURFACE_STYLE_FILL_AREA ( #6887 ) ;
#7371 = VECTOR ( 'NONE', #6977, 1000.000000000000000 ) ;
#7372 = CARTESIAN_POINT ( 'NONE',  ( 6.187144687173720570, -58.64655194120005177, 0.3691021985165400809 ) ) ;
#7373 = DIRECTION ( 'NONE',  ( -5.715354789845005112E-18, -9.999836672264339449E-16, 1.000000000000000000 ) ) ;
#7374 = CIRCLE ( 'NONE', #4138, 3.300000000000000711 ) ;
#7375 = CIRCLE ( 'NONE', #4634, 1.000000000000001998 ) ;
#7376 = DIRECTION ( 'NONE',  ( 0.000000000000000000, 0.000000000000000000, -1.000000000000000000 ) ) ;
#7377 = CARTESIAN_POINT ( 'NONE',  ( 39.97800414936823188, -95.26063634933134949, -3.001370543551635794 ) ) ;
#7378 = ORIENTED_EDGE ( 'NONE', *, *, #6115, .F. ) ;
#7379 = AXIS2_PLACEMENT_3D ( 'NONE', #5203, #6470, #1316 ) ;
#7380 = EDGE_CURVE ( 'NONE', #4908, #936, #556, .T. ) ;
#7381 = CARTESIAN_POINT ( 'NONE',  ( -33.25476684253234794, 13.81160679460617757, -1.499999999999986899 ) ) ;
#7382 = EDGE_CURVE ( 'NONE', #1758, #1972, #1941, .T. ) ;
#7383 = CARTESIAN_POINT ( 'NONE',  ( -16.44258018226587836, 7.261459853215404436, -0.3999035282155121718 ) ) ;
#7384 = DIRECTION ( 'NONE',  ( 0.9999836672264332815, -0.005715354789845002517, 0.000000000000000000 ) ) ;
#7385 = VECTOR ( 'NONE', #932, 1000.000000000000000 ) ;
#7386 = CARTESIAN_POINT ( 'NONE',  ( 5.904685685680689744, -64.36828453093134783, 1.045689304822035037 ) ) ;
#7387 = CARTESIAN_POINT ( 'NONE',  ( 43.89994888609457035, -93.87291691326068133, 2.999999999999906297 ) ) ;
#7388 = ORIENTED_EDGE ( 'NONE', *, *, #5784, .F. ) ;
#7389 = CARTESIAN_POINT ( 'NONE',  ( -20.16480223318149356, 14.61937842657788167, 0.006154456448484012937 ) ) ;
#7390 = CARTESIAN_POINT ( 'NONE',  ( 2.735691016399460107, -56.17047939608508500, 0.9718516700694501687 ) ) ;
#7391 = FACE_OUTER_BOUND ( 'NONE', #3665, .T. ) ;
#7392 = ADVANCED_FACE ( 'NONE', ( #1056 ), #2216, .T. ) ;
#7393 = CARTESIAN_POINT ( 'NONE',  ( 43.45632180942044442, -94.90042465344848210, 2.999999999999905409 ) ) ;
#7394 = CARTESIAN_POINT ( 'NONE',  ( 4.890810490072590611, -59.09042288871975757, -0.8837144134564199893 ) ) ;
#7395 = CARTESIAN_POINT ( 'NONE',  ( 27.81637696285268291, -34.74025023524533395, 3.614652068524565109 ) ) ;
#7396 = CYLINDRICAL_SURFACE ( 'NONE', #1330, 0.7499999999999994449 ) ;
#7397 = CARTESIAN_POINT ( 'NONE',  ( 2.440761905804889942, -65.30842328614467363, 1.105894752426585415 ) ) ;
#7398 = ORIENTED_EDGE ( 'NONE', *, *, #619, .F. ) ;
#7399 = ORIENTED_EDGE ( 'NONE', *, *, #6459, .F. ) ;
#7400 = ORIENTED_EDGE ( 'NONE', *, *, #1280, .F. ) ;
#7401 = DIRECTION ( 'NONE',  ( -5.715354789860003484E-18, -9.999836672264337477E-16, 1.000000000000000000 ) ) ;
#7402 = ORIENTED_EDGE ( 'NONE', *, *, #5359, .T. ) ;
#7403 = CARTESIAN_POINT ( 'NONE',  ( 18.31184849395310721, -40.14648560017521106, 3.999999999999959144 ) ) ;
#7404 = CARTESIAN_POINT ( 'NONE',  ( 12.15447797363371052, 11.01039466689934798, -3.299999999999988720 ) ) ;
#7405 = CARTESIAN_POINT ( 'NONE',  ( -7.067610632470020526, -58.47094543896879060, 0.9162228916581999227 ) ) ;
#7406 = ORIENTED_EDGE ( 'NONE', *, *, #5712, .T. ) ;
#7407 = ORIENTED_EDGE ( 'NONE', *, *, #5919, .F. ) ;
#7408 = ORIENTED_EDGE ( 'NONE', *, *, #4137, .F. ) ;
#7409 = DIRECTION ( 'NONE',  ( -0.9492883822130750993, 0.3144066910790586089, 0.000000000000000000 ) ) ;
#7410 = DIRECTION ( 'NONE',  ( 5.715354789845005112E-18, 9.999836672264339449E-16, -1.000000000000000000 ) ) ;
#7411 = DIRECTION ( 'NONE',  ( 0.9999836672264332815, -0.005715354789859183882, 0.000000000000000000 ) ) ;
#7412 = CARTESIAN_POINT ( 'NONE',  ( -33.25476684253263215, 13.81160679460551677, -2.250000000002000178 ) ) ;
#7413 = DIRECTION ( 'NONE',  ( -0.8688689365825387201, -0.4950421911735688463, -4.999999999999993486E-16 ) ) ;
#7414 = DIRECTION ( 'NONE',  ( -0.9999836672264332815, 0.005715354789859956701, 0.000000000000000000 ) ) ;
#7415 = VERTEX_POINT ( 'NONE', #1690 ) ;
#7416 = EDGE_CURVE ( 'NONE', #7431, #6609, #2187, .T. ) ;
#7417 = CARTESIAN_POINT ( 'NONE',  ( 18.49916120972755351, -39.46430250869197209, 3.999999999999961808 ) ) ;
#7418 = PLANE ( 'NONE',  #1734 ) ;
#7419 = DIRECTION ( 'NONE',  ( -5.715354789845005112E-18, -9.999836672264339449E-16, 1.000000000000000000 ) ) ;
#7420 = CARTESIAN_POINT ( 'NONE',  ( -6.733769393910259637, -61.90091566649680743, 1.831080987178660191 ) ) ;
#7421 = DIRECTION ( 'NONE',  ( -0.9721221936972339606, -0.2344748185227520099, 0.000000000000000000 ) ) ;
#7422 = VERTEX_POINT ( 'NONE', #5769 ) ;
#7423 = EDGE_CURVE ( 'NONE', #577, #937, #1618, .T. ) ;
#7424 = ADVANCED_FACE ( 'NONE', ( #1092 ), #637, .T. ) ;
#7425 = DIRECTION ( 'NONE',  ( 5.715354789845005112E-18, 9.999836672264339449E-16, -1.000000000000000000 ) ) ;
#7426 = CARTESIAN_POINT ( 'NONE',  ( 18.29784290781275757, -40.16735820407432556, -0.8913619061384294717 ) ) ;
#7427 = LINE ( 'NONE', #4050, #6304 ) ;
#7428 = CARTESIAN_POINT ( 'NONE',  ( 5.191094514348209898, -57.61090315545595786, 2.520404771314449732 ) ) ;
#7429 = LINE ( 'NONE', #3442, #3636 ) ;
#7430 = CARTESIAN_POINT ( 'NONE',  ( -32.93157973858376408, 14.54341967768581512, 1.435496648130876646E-14 ) ) ;
#7431 = VERTEX_POINT ( 'NONE', #2254 ) ;
#7432 = ADVANCED_FACE ( 'NONE', ( #6929 ), #3986, .T. ) ;
#7433 = EDGE_LOOP ( 'NONE', ( #5166, #2619 ) ) ;
#7434 = VERTEX_POINT ( 'NONE', #1208 ) ;
#7435 = CARTESIAN_POINT ( 'NONE',  ( 18.06432739836606771, -39.71205113188411673, 3.132117705585802270 ) ) ;
#7436 = ORIENTED_EDGE ( 'NONE', *, *, #1631, .T. ) ;
#7437 = FACE_OUTER_BOUND ( 'NONE', #2847, .T. ) ;
#7438 = DIRECTION ( 'NONE',  ( 0.5818022356294096920, -0.8133302887613499399, -8.099917986277619058E-16 ) ) ;
#7439 = FACE_OUTER_BOUND ( 'NONE', #559, .T. ) ;
#7440 = CARTESIAN_POINT ( 'NONE',  ( 3.193531232915834739, -66.77446787883670254, 1.223174286645849929 ) ) ;
#7441 = ORIENTED_EDGE ( 'NONE', *, *, #2504, .T. ) ;
#7442 = VERTEX_POINT ( 'NONE', #3489 ) ;
#7443 = AXIS2_PLACEMENT_3D ( 'NONE', #7004, #752, #194 ) ;
#7444 = DIRECTION ( 'NONE',  ( -0.03652191451860400950, -0.9993328523369456873, -9.995252661588299226E-16 ) ) ;
#7445 = NEXT_ASSEMBLY_USAGE_OCCURRENCE ( 'NAUO1', ' ', ' ', #5025, #1226, $ ) ;
#7446 = NEXT_ASSEMBLY_USAGE_OCCURRENCE ( 'NAUO2', ' ', ' ', #5025, #4117, $ ) ;
#7447 = NEXT_ASSEMBLY_USAGE_OCCURRENCE ( 'NAUO3', ' ', ' ', #5025, #4256, $ ) ;
#7448 = NEXT_ASSEMBLY_USAGE_OCCURRENCE ( 'NAUO4', ' ', ' ', #5025, #5465, $ ) ;
#7449 = NEXT_ASSEMBLY_USAGE_OCCURRENCE ( 'NAUO5', ' ', ' ', #5025, #6489, $ ) ;
#7450 = NEXT_ASSEMBLY_USAGE_OCCURRENCE ( 'NAUO6', ' ', ' ', #5025, #4117, $ ) ;
ENDSEC;
END-ISO-10303-21;
